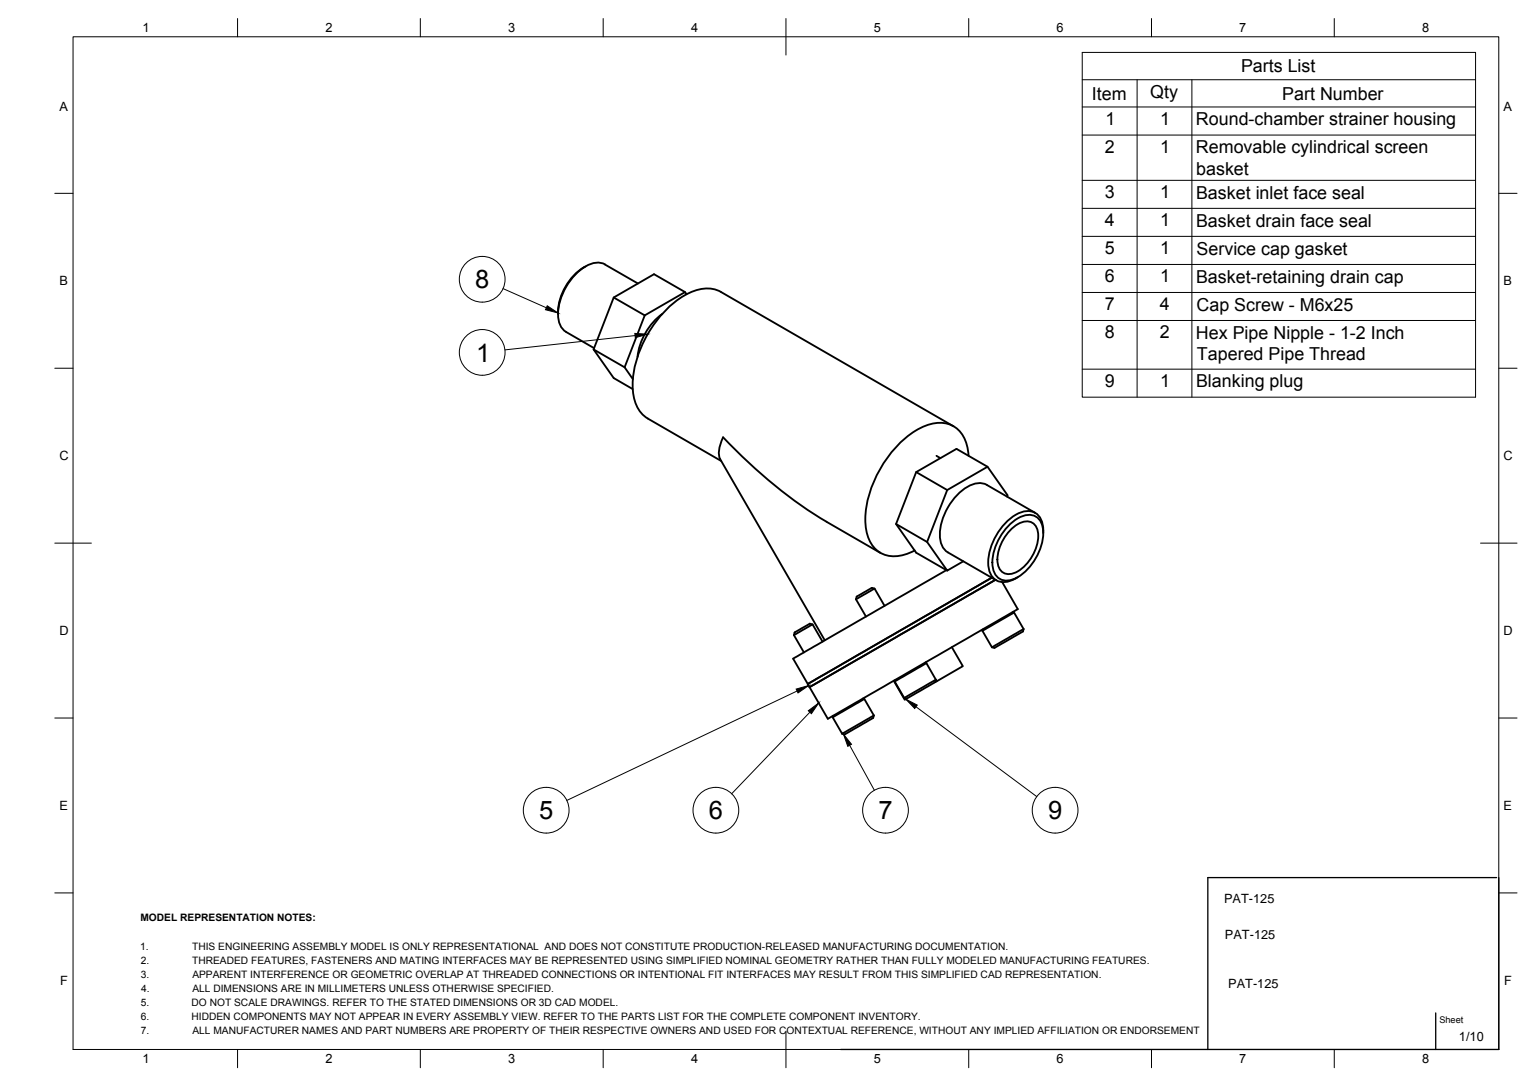
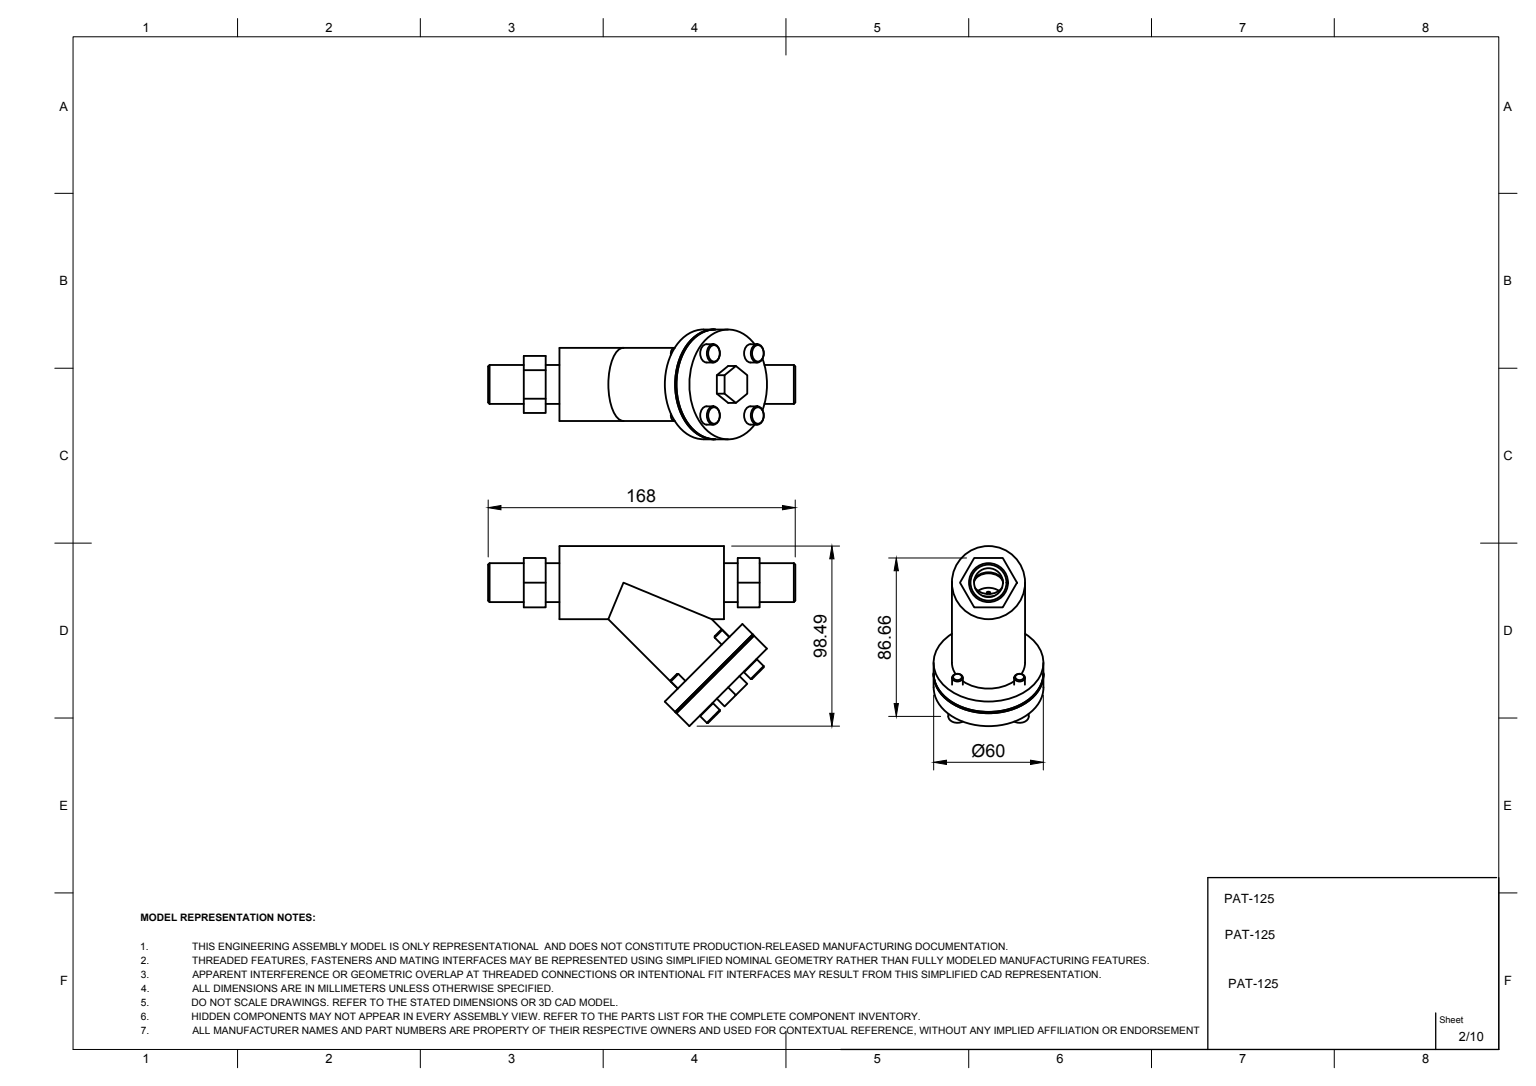
ISO-10303-21;
HEADER;
/* Generated by software containing ST-Developer
 * from STEP Tools, Inc. (www.steptools.com) 
 */

FILE_DESCRIPTION(
/* description */ ('Y-strainer with drain'),
/* implementation_level */ '2;1');

FILE_NAME(
/* name */ 'PAT-125',
/* time_stamp */ '2026-10-28T00:41:55-07:00',
/* author */ (''),
/* organization */ (''),
/* preprocessor_version */ 'ST-DEVELOPER v20.2',
/* originating_system */ 'Autodesk Translation Framework v15.17.0.0',
/* authorisation */ '');

FILE_SCHEMA (('AUTOMOTIVE_DESIGN { 1 0 10303 214 3 1 1 }'));
ENDSEC;

DATA;
#10=MECHANICAL_DESIGN_GEOMETRIC_PRESENTATION_REPRESENTATION('',(#93,#94,
#95,#96,#97,#98,#99,#100,#101),#8864);
#11=ITEM_DEFINED_TRANSFORMATION($,$,#3495,#3757);
#12=ITEM_DEFINED_TRANSFORMATION($,$,#3557,#3758);
#13=ITEM_DEFINED_TRANSFORMATION($,$,#3630,#3759);
#14=ITEM_DEFINED_TRANSFORMATION($,$,#3639,#3760);
#15=ITEM_DEFINED_TRANSFORMATION($,$,#3648,#3761);
#16=ITEM_DEFINED_TRANSFORMATION($,$,#3669,#3762);
#17=ITEM_DEFINED_TRANSFORMATION($,$,#3694,#3763);
#18=ITEM_DEFINED_TRANSFORMATION($,$,#3694,#3764);
#19=ITEM_DEFINED_TRANSFORMATION($,$,#3694,#3765);
#20=ITEM_DEFINED_TRANSFORMATION($,$,#3694,#3766);
#21=ITEM_DEFINED_TRANSFORMATION($,$,#3720,#3767);
#22=ITEM_DEFINED_TRANSFORMATION($,$,#3720,#3768);
#23=ITEM_DEFINED_TRANSFORMATION($,$,#3744,#3769);
#24=ITEM_DEFINED_TRANSFORMATION($,$,#3494,#3770);
#25=(
REPRESENTATION_RELATIONSHIP($,$,#8907,#8906)
REPRESENTATION_RELATIONSHIP_WITH_TRANSFORMATION(#11)
SHAPE_REPRESENTATION_RELATIONSHIP()
);
#26=(
REPRESENTATION_RELATIONSHIP($,$,#8908,#8906)
REPRESENTATION_RELATIONSHIP_WITH_TRANSFORMATION(#12)
SHAPE_REPRESENTATION_RELATIONSHIP()
);
#27=(
REPRESENTATION_RELATIONSHIP($,$,#8909,#8906)
REPRESENTATION_RELATIONSHIP_WITH_TRANSFORMATION(#13)
SHAPE_REPRESENTATION_RELATIONSHIP()
);
#28=(
REPRESENTATION_RELATIONSHIP($,$,#8910,#8906)
REPRESENTATION_RELATIONSHIP_WITH_TRANSFORMATION(#14)
SHAPE_REPRESENTATION_RELATIONSHIP()
);
#29=(
REPRESENTATION_RELATIONSHIP($,$,#8911,#8906)
REPRESENTATION_RELATIONSHIP_WITH_TRANSFORMATION(#15)
SHAPE_REPRESENTATION_RELATIONSHIP()
);
#30=(
REPRESENTATION_RELATIONSHIP($,$,#8912,#8906)
REPRESENTATION_RELATIONSHIP_WITH_TRANSFORMATION(#16)
SHAPE_REPRESENTATION_RELATIONSHIP()
);
#31=(
REPRESENTATION_RELATIONSHIP($,$,#8913,#8906)
REPRESENTATION_RELATIONSHIP_WITH_TRANSFORMATION(#17)
SHAPE_REPRESENTATION_RELATIONSHIP()
);
#32=(
REPRESENTATION_RELATIONSHIP($,$,#8913,#8906)
REPRESENTATION_RELATIONSHIP_WITH_TRANSFORMATION(#18)
SHAPE_REPRESENTATION_RELATIONSHIP()
);
#33=(
REPRESENTATION_RELATIONSHIP($,$,#8913,#8906)
REPRESENTATION_RELATIONSHIP_WITH_TRANSFORMATION(#19)
SHAPE_REPRESENTATION_RELATIONSHIP()
);
#34=(
REPRESENTATION_RELATIONSHIP($,$,#8913,#8906)
REPRESENTATION_RELATIONSHIP_WITH_TRANSFORMATION(#20)
SHAPE_REPRESENTATION_RELATIONSHIP()
);
#35=(
REPRESENTATION_RELATIONSHIP($,$,#8914,#8906)
REPRESENTATION_RELATIONSHIP_WITH_TRANSFORMATION(#21)
SHAPE_REPRESENTATION_RELATIONSHIP()
);
#36=(
REPRESENTATION_RELATIONSHIP($,$,#8914,#8906)
REPRESENTATION_RELATIONSHIP_WITH_TRANSFORMATION(#22)
SHAPE_REPRESENTATION_RELATIONSHIP()
);
#37=(
REPRESENTATION_RELATIONSHIP($,$,#8915,#8906)
REPRESENTATION_RELATIONSHIP_WITH_TRANSFORMATION(#23)
SHAPE_REPRESENTATION_RELATIONSHIP()
);
#38=(
REPRESENTATION_RELATIONSHIP($,$,#8906,#8905)
REPRESENTATION_RELATIONSHIP_WITH_TRANSFORMATION(#24)
SHAPE_REPRESENTATION_RELATIONSHIP()
);
#39=CONTEXT_DEPENDENT_SHAPE_REPRESENTATION(#25,#8891);
#40=CONTEXT_DEPENDENT_SHAPE_REPRESENTATION(#26,#8892);
#41=CONTEXT_DEPENDENT_SHAPE_REPRESENTATION(#27,#8893);
#42=CONTEXT_DEPENDENT_SHAPE_REPRESENTATION(#28,#8894);
#43=CONTEXT_DEPENDENT_SHAPE_REPRESENTATION(#29,#8895);
#44=CONTEXT_DEPENDENT_SHAPE_REPRESENTATION(#30,#8896);
#45=CONTEXT_DEPENDENT_SHAPE_REPRESENTATION(#31,#8897);
#46=CONTEXT_DEPENDENT_SHAPE_REPRESENTATION(#32,#8898);
#47=CONTEXT_DEPENDENT_SHAPE_REPRESENTATION(#33,#8899);
#48=CONTEXT_DEPENDENT_SHAPE_REPRESENTATION(#34,#8900);
#49=CONTEXT_DEPENDENT_SHAPE_REPRESENTATION(#35,#8901);
#50=CONTEXT_DEPENDENT_SHAPE_REPRESENTATION(#36,#8902);
#51=CONTEXT_DEPENDENT_SHAPE_REPRESENTATION(#37,#8903);
#52=CONTEXT_DEPENDENT_SHAPE_REPRESENTATION(#38,#8904);
#53=NEXT_ASSEMBLY_USAGE_OCCURRENCE('Round-chamber strainer housing:1',
'Round-chamber strainer housing:1','Round-chamber strainer housing:1',#8918,
#8919,'Round-chamber strainer housing:1');
#54=NEXT_ASSEMBLY_USAGE_OCCURRENCE(
'Removable cylindrical screen basket:1',
'Removable cylindrical screen basket:1',
'Removable cylindrical screen basket:1',#8918,#8920,
'Removable cylindrical screen basket:1');
#55=NEXT_ASSEMBLY_USAGE_OCCURRENCE('Basket inlet face seal:1',
'Basket inlet face seal:1','Basket inlet face seal:1',#8918,#8921,
'Basket inlet face seal:1');
#56=NEXT_ASSEMBLY_USAGE_OCCURRENCE('Basket drain face seal:1',
'Basket drain face seal:1','Basket drain face seal:1',#8918,#8922,
'Basket drain face seal:1');
#57=NEXT_ASSEMBLY_USAGE_OCCURRENCE('Service cap gasket:1',
'Service cap gasket:1','Service cap gasket:1',#8918,#8923,
'Service cap gasket:1');
#58=NEXT_ASSEMBLY_USAGE_OCCURRENCE('Basket-retaining drain cap:1',
'Basket-retaining drain cap:1','Basket-retaining drain cap:1',#8918,#8924,
'Basket-retaining drain cap:1');
#59=NEXT_ASSEMBLY_USAGE_OCCURRENCE('Cap Screw - M6x25:2',
'Cap Screw - M6x25:2','Cap Screw - M6x25:2',#8918,#8925,
'Cap Screw - M6x25:2');
#60=NEXT_ASSEMBLY_USAGE_OCCURRENCE('Cap Screw - M6x25:3',
'Cap Screw - M6x25:3','Cap Screw - M6x25:3',#8918,#8925,
'Cap Screw - M6x25:3');
#61=NEXT_ASSEMBLY_USAGE_OCCURRENCE('Cap Screw - M6x25:4',
'Cap Screw - M6x25:4','Cap Screw - M6x25:4',#8918,#8925,
'Cap Screw - M6x25:4');
#62=NEXT_ASSEMBLY_USAGE_OCCURRENCE('Cap Screw - M6x25:5',
'Cap Screw - M6x25:5','Cap Screw - M6x25:5',#8918,#8925,
'Cap Screw - M6x25:5');
#63=NEXT_ASSEMBLY_USAGE_OCCURRENCE(
'Hex Pipe Nipple - 1-2 Inch Tapered Pipe Thread:2',
'Hex Pipe Nipple - 1-2 Inch Tapered Pipe Thread:2',
'Hex Pipe Nipple - 1-2 Inch Tapered Pipe Thread:2',#8918,#8926,
'Hex Pipe Nipple - 1-2 Inch Tapered Pipe Thread:2');
#64=NEXT_ASSEMBLY_USAGE_OCCURRENCE(
'Hex Pipe Nipple - 1-2 Inch Tapered Pipe Thread:3',
'Hex Pipe Nipple - 1-2 Inch Tapered Pipe Thread:3',
'Hex Pipe Nipple - 1-2 Inch Tapered Pipe Thread:3',#8918,#8926,
'Hex Pipe Nipple - 1-2 Inch Tapered Pipe Thread:3');
#65=NEXT_ASSEMBLY_USAGE_OCCURRENCE('Blanking plug:2','Blanking plug:2',
'Blanking plug:2',#8918,#8927,'Blanking plug:2');
#66=NEXT_ASSEMBLY_USAGE_OCCURRENCE(
'Strainer housing basket seals cap and fittings:1',
'Strainer housing basket seals cap and fittings:1',
'Strainer housing basket seals cap and fittings:1',#8917,#8918,
'Strainer housing basket seals cap and fittings:1');
#67=ORIENTED_CLOSED_SHELL('',*,#3390,.F.);
#68=CONICAL_SURFACE('',#3697,0.475,0.785398163397449);
#69=CONICAL_SURFACE('',#3701,0.485,0.785398163397448);
#70=CONICAL_SURFACE('',#3705,0.31,0.463647609000806);
#71=CONICAL_SURFACE('',#3709,0.27,0.785398163397448);
#72=CONICAL_SURFACE('',#3736,1.025,0.785398163397448);
#73=CONICAL_SURFACE('',#3739,1.025,0.785398163397448);
#74=BREP_WITH_VOIDS('Body1',#3389,(#67));
#75=SHAPE_REPRESENTATION_RELATIONSHIP('SRR','None',#8907,#84);
#76=SHAPE_REPRESENTATION_RELATIONSHIP('SRR','None',#8908,#85);
#77=SHAPE_REPRESENTATION_RELATIONSHIP('SRR','None',#8909,#86);
#78=SHAPE_REPRESENTATION_RELATIONSHIP('SRR','None',#8910,#87);
#79=SHAPE_REPRESENTATION_RELATIONSHIP('SRR','None',#8911,#88);
#80=SHAPE_REPRESENTATION_RELATIONSHIP('SRR','None',#8912,#89);
#81=SHAPE_REPRESENTATION_RELATIONSHIP('SRR','None',#8913,#90);
#82=SHAPE_REPRESENTATION_RELATIONSHIP('SRR','None',#8914,#91);
#83=SHAPE_REPRESENTATION_RELATIONSHIP('SRR','None',#8915,#92);
#84=ADVANCED_BREP_SHAPE_REPRESENTATION('',(#102),#8855);
#85=ADVANCED_BREP_SHAPE_REPRESENTATION('',(#103),#8856);
#86=ADVANCED_BREP_SHAPE_REPRESENTATION('',(#104),#8857);
#87=ADVANCED_BREP_SHAPE_REPRESENTATION('',(#105),#8858);
#88=ADVANCED_BREP_SHAPE_REPRESENTATION('',(#106),#8859);
#89=ADVANCED_BREP_SHAPE_REPRESENTATION('',(#107),#8860);
#90=ADVANCED_BREP_SHAPE_REPRESENTATION('',(#74),#8861);
#91=ADVANCED_BREP_SHAPE_REPRESENTATION('',(#108),#8862);
#92=ADVANCED_BREP_SHAPE_REPRESENTATION('',(#109),#8863);
#93=STYLED_ITEM('',(#9012),#102);
#94=STYLED_ITEM('',(#9026),#103);
#95=STYLED_ITEM('',(#9040),#104);
#96=STYLED_ITEM('',(#9040),#105);
#97=STYLED_ITEM('',(#9019),#106);
#98=STYLED_ITEM('',(#9019),#107);
#99=STYLED_ITEM('',(#9040),#74);
#100=STYLED_ITEM('',(#9019),#108);
#101=STYLED_ITEM('',(#9047),#109);
#102=MANIFOLD_SOLID_BREP('Body1',#3383);
#103=MANIFOLD_SOLID_BREP('Body1',#3384);
#104=MANIFOLD_SOLID_BREP('Body1',#3385);
#105=MANIFOLD_SOLID_BREP('Body1',#3386);
#106=MANIFOLD_SOLID_BREP('Body1',#3387);
#107=MANIFOLD_SOLID_BREP('Body1',#3388);
#108=MANIFOLD_SOLID_BREP('Body1',#3391);
#109=MANIFOLD_SOLID_BREP('Body1',#3392);
#110=B_SPLINE_CURVE_WITH_KNOTS('',3,(#4530,#4531,#4532,#4533,#4534,#4535,
#4536,#4537,#4538,#4539,#4540,#4541,#4542,#4543,#4544,#4545,#4546,#4547,
#4548,#4549),.UNSPECIFIED.,.F.,.F.,(4,2,2,2,2,2,2,2,2,4),(-4.14934014091753,
-3.99654801890952,-3.81097439305959,-3.62540076720966,-3.2542535155098,
-2.75110698726675,-2.2479604590237,-1.9375436083893,-1.7823351830721,-1.6271267577549),
 .UNSPECIFIED.);
#111=B_SPLINE_CURVE_WITH_KNOTS('',3,(#4550,#4551,#4552,#4553,#4554,#4555,
#4556,#4557,#4558,#4559,#4560,#4561,#4562,#4563,#4564,#4565,#4566,#4567,
#4568,#4569,#4570),.UNSPECIFIED.,.F.,.F.,(4,2,2,2,2,3,2,2,2,4),(-1.6271267577549,
-1.4719183324377,-1.3167099071205,-1.00629305648611,-0.503146528243052,
0.,0.371147251699857,0.556720877549785,0.742294503399713,0.895086625004965),
 .UNSPECIFIED.);
#112=B_SPLINE_CURVE_WITH_KNOTS('',3,(#4581,#4582,#4583,#4584,#4585,#4586,
#4587,#4588,#4589,#4590),.UNSPECIFIED.,.F.,.F.,(4,2,2,2,4),(1.74412062919654,
1.93171537626907,2.23482107464905,2.53792677302904,2.72552152010157),
 .UNSPECIFIED.);
#113=B_SPLINE_CURVE_WITH_KNOTS('',3,(#4608,#4609,#4610,#4611,#4612,#4613,
#4614,#4615,#4616,#4617,#4618,#4619,#4620,#4621,#4622,#4623,#4624,#4625,
#4626),.UNSPECIFIED.,.F.,.F.,(4,2,2,2,2,3,2,2,4),(-1.08793576529359,-1.02464359039736,
-0.589129183459348,-0.223538305364611,-0.111769152682306,0.,0.0571948520978316,
0.114389704195663,0.138769598257235),.UNSPECIFIED.);
#114=B_SPLINE_CURVE_WITH_KNOTS('',3,(#4628,#4629,#4630,#4631,#4632,#4633,
#4634,#4635,#4636,#4637,#4638,#4639,#4640,#4641,#4642,#4643,#4644,#4645),
 .UNSPECIFIED.,.F.,.F.,(4,2,2,2,2,2,2,2,4),(2.32433792360818,2.34871781766975,
2.40591266976758,2.46310752186541,2.57487667454772,2.68664582723002,3.05223670532476,
3.48775111226277,3.551043287159),.UNSPECIFIED.);
#115=B_SPLINE_CURVE_WITH_KNOTS('',3,(#4698,#4699,#4700,#4701,#4702,#4703,
#4704,#4705,#4706,#4707),.UNSPECIFIED.,.F.,.F.,(4,2,2,2,4),(0.,0.0376910486946462,
0.0753820973892924,0.113073058602025,0.150764019814758),.UNSPECIFIED.);
#116=B_SPLINE_CURVE_WITH_KNOTS('',3,(#4708,#4709,#4710,#4711,#4712,#4713,
#4714,#4715,#4716,#4717,#4718,#4719,#4720,#4721,#4722,#4723,#4724,#4725,
#4726,#4727,#4728,#4729,#4730,#4731,#4732,#4733),.UNSPECIFIED.,.F.,.F.,
(4,2,2,2,2,2,2,2,2,2,2,2,4),(0.150764019814758,0.188454981027491,0.226145942240224,
0.26383699093487,0.301528039629516,0.339219088324162,0.376910137018808,
0.414601098231541,0.452292059444274,0.489983020657007,0.527673981869739,
0.565365030564385,0.603056079259032),.UNSPECIFIED.);
#117=B_SPLINE_CURVE_WITH_KNOTS('',3,(#4737,#4738,#4739,#4740,#4741,#4742,
#4743,#4744,#4745,#4746,#4747,#4748,#4749,#4750,#4751,#4752,#4753,#4754,
#4755,#4756,#4757,#4758,#4759,#4760,#4761,#4762),.UNSPECIFIED.,.F.,.F.,
(4,2,2,2,2,2,2,2,2,2,2,2,4),(0.,0.0376957822030297,0.0753915644060595,0.113087218301784,
0.150782872197509,0.188478526093234,0.226174179988958,0.263869962191988,
0.301565744395018,0.339261526598047,0.376957308801077,0.414652962696802,
0.452348616592527),.UNSPECIFIED.);
#118=B_SPLINE_CURVE_WITH_KNOTS('',3,(#4763,#4764,#4765,#4766,#4767,#4768,
#4769,#4770,#4771,#4772),.UNSPECIFIED.,.F.,.F.,(4,2,2,2,4),(0.452348616592527,
0.490044270488251,0.527739924383976,0.565435706587006,0.603131488790035),
 .UNSPECIFIED.);
#119=B_SPLINE_CURVE_WITH_KNOTS('',3,(#4776,#4777,#4778,#4779,#4780,#4781,
#4782,#4783,#4784,#4785),.UNSPECIFIED.,.F.,.F.,(4,2,2,2,4),(0.,0.0376957822030298,
0.0753915644060595,0.113087218301784,0.150782872197509),.UNSPECIFIED.);
#120=B_SPLINE_CURVE_WITH_KNOTS('',3,(#4786,#4787,#4788,#4789,#4790,#4791,
#4792,#4793,#4794,#4795,#4796,#4797,#4798,#4799,#4800,#4801,#4802,#4803,
#4804,#4805,#4806,#4807,#4808,#4809,#4810,#4811),.UNSPECIFIED.,.F.,.F.,
(4,2,2,2,2,2,2,2,2,2,2,2,4),(0.150782872197509,0.188478526093234,0.226174179988958,
0.263869962191988,0.301565744395018,0.339261526598047,0.376957308801077,
0.414652962696802,0.452348616592526,0.490044270488251,0.527739924383976,
0.565435706587005,0.603131488790035),.UNSPECIFIED.);
#121=B_SPLINE_CURVE_WITH_KNOTS('',3,(#4815,#4816,#4817,#4818,#4819,#4820,
#4821,#4822,#4823,#4824,#4825,#4826,#4827,#4828,#4829,#4830,#4831,#4832,
#4833,#4834,#4835,#4836,#4837,#4838,#4839,#4840),.UNSPECIFIED.,.F.,.F.,
(4,2,2,2,2,2,2,2,2,2,2,2,4),(0.,0.0376910486946462,0.0753820973892924,0.113073058602025,
0.150764019814758,0.188454981027491,0.226145942240224,0.26383699093487,
0.301528039629516,0.339219088324162,0.376910137018808,0.414601098231541,
0.452292059444274),.UNSPECIFIED.);
#122=B_SPLINE_CURVE_WITH_KNOTS('',3,(#4841,#4842,#4843,#4844,#4845,#4846,
#4847,#4848,#4849,#4850),.UNSPECIFIED.,.F.,.F.,(4,2,2,2,4),(0.452292059444274,
0.489983020657006,0.527673981869739,0.565365030564385,0.603056079259032),
 .UNSPECIFIED.);
#123=B_SPLINE_CURVE_WITH_KNOTS('',3,(#4854,#4855,#4856,#4857,#4858,#4859,
#4860,#4861,#4862,#4863),.UNSPECIFIED.,.F.,.F.,(4,2,2,2,4),(0.,0.0376910486946458,
0.0753820973892915,0.113073058602024,0.150764019814757),.UNSPECIFIED.);
#124=B_SPLINE_CURVE_WITH_KNOTS('',3,(#4864,#4865,#4866,#4867,#4868,#4869,
#4870,#4871,#4872,#4873,#4874,#4875,#4876,#4877,#4878,#4879,#4880,#4881,
#4882,#4883,#4884,#4885,#4886,#4887,#4888,#4889),.UNSPECIFIED.,.F.,.F.,
(4,2,2,2,2,2,2,2,2,2,2,2,4),(0.150764019814757,0.18845498102749,0.226145942240223,
0.263836990934869,0.301528039629515,0.339219088324161,0.376910137018807,
0.41460109823154,0.452292059444273,0.489983020657006,0.527673981869738,
0.565365030564384,0.603056079259031),.UNSPECIFIED.);
#125=B_SPLINE_CURVE_WITH_KNOTS('',3,(#4893,#4894,#4895,#4896,#4897,#4898,
#4899,#4900,#4901,#4902,#4903,#4904,#4905,#4906,#4907,#4908,#4909,#4910,
#4911,#4912,#4913,#4914,#4915,#4916,#4917,#4918),.UNSPECIFIED.,.F.,.F.,
(4,2,2,2,2,2,2,2,2,2,2,2,4),(0.,0.0376957822030297,0.0753915644060595,0.113087218301784,
0.150782872197509,0.188478526093234,0.226174179988958,0.263869962191988,
0.301565744395018,0.339261526598047,0.376957308801077,0.414652962696802,
0.452348616592527),.UNSPECIFIED.);
#126=B_SPLINE_CURVE_WITH_KNOTS('',3,(#4919,#4920,#4921,#4922,#4923,#4924,
#4925,#4926,#4927,#4928),.UNSPECIFIED.,.F.,.F.,(4,2,2,2,4),(0.452348616592527,
0.490044270488251,0.527739924383976,0.565435706587006,0.603131488790035),
 .UNSPECIFIED.);
#127=B_SPLINE_CURVE_WITH_KNOTS('',3,(#4932,#4933,#4934,#4935,#4936,#4937,
#4938,#4939,#4940,#4941),.UNSPECIFIED.,.F.,.F.,(4,2,2,2,4),(0.,0.0376957822030298,
0.0753915644060595,0.113087218301784,0.150782872197509),.UNSPECIFIED.);
#128=B_SPLINE_CURVE_WITH_KNOTS('',3,(#4942,#4943,#4944,#4945,#4946,#4947,
#4948,#4949,#4950,#4951,#4952,#4953,#4954,#4955,#4956,#4957,#4958,#4959,
#4960,#4961,#4962,#4963,#4964,#4965,#4966,#4967),.UNSPECIFIED.,.F.,.F.,
(4,2,2,2,2,2,2,2,2,2,2,2,4),(0.150782872197509,0.188478526093234,0.226174179988958,
0.263869962191988,0.301565744395018,0.339261526598047,0.376957308801077,
0.414652962696802,0.452348616592526,0.490044270488251,0.527739924383976,
0.565435706587005,0.603131488790035),.UNSPECIFIED.);
#129=B_SPLINE_CURVE_WITH_KNOTS('',3,(#4971,#4972,#4973,#4974,#4975,#4976,
#4977,#4978,#4979,#4980,#4981,#4982,#4983,#4984,#4985,#4986,#4987,#4988,
#4989,#4990,#4991,#4992,#4993,#4994,#4995,#4996),.UNSPECIFIED.,.F.,.F.,
(4,2,2,2,2,2,2,2,2,2,2,2,4),(0.,0.0376910486946462,0.0753820973892924,0.113073058602025,
0.150764019814758,0.188454981027491,0.226145942240224,0.26383699093487,
0.301528039629516,0.339219088324161,0.376910137018807,0.41460109823154,
0.452292059444273),.UNSPECIFIED.);
#130=B_SPLINE_CURVE_WITH_KNOTS('',3,(#4997,#4998,#4999,#5000,#5001,#5002,
#5003,#5004,#5005,#5006),.UNSPECIFIED.,.F.,.F.,(4,2,2,2,4),(0.452292059444273,
0.489983020657006,0.527673981869739,0.565365030564385,0.603056079259031),
 .UNSPECIFIED.);
#131=B_SPLINE_CURVE_WITH_KNOTS('',3,(#5010,#5011,#5012,#5013,#5014,#5015,
#5016,#5017,#5018,#5019),.UNSPECIFIED.,.F.,.F.,(4,2,2,2,4),(0.,0.0376910486946464,
0.0753820973892928,0.113073058602026,0.150764019814759),.UNSPECIFIED.);
#132=B_SPLINE_CURVE_WITH_KNOTS('',3,(#5020,#5021,#5022,#5023,#5024,#5025,
#5026,#5027,#5028,#5029,#5030,#5031,#5032,#5033,#5034,#5035,#5036,#5037,
#5038,#5039,#5040,#5041,#5042,#5043,#5044,#5045),.UNSPECIFIED.,.F.,.F.,
(4,2,2,2,2,2,2,2,2,2,2,2,4),(0.150764019814759,0.188454981027492,0.226145942240225,
0.263836990934871,0.301528039629517,0.339219088324163,0.37691013701881,
0.414601098231543,0.452292059444276,0.489983020657009,0.527673981869742,
0.565365030564388,0.603056079259034),.UNSPECIFIED.);
#133=B_SPLINE_CURVE_WITH_KNOTS('',3,(#5049,#5050,#5051,#5052,#5053,#5054,
#5055,#5056,#5057,#5058,#5059,#5060,#5061,#5062,#5063,#5064,#5065,#5066,
#5067,#5068,#5069,#5070,#5071,#5072,#5073,#5074),.UNSPECIFIED.,.F.,.F.,
(4,2,2,2,2,2,2,2,2,2,2,2,4),(0.,0.0376957822030297,0.0753915644060594,0.113087218301785,
0.15078287219751,0.188478526093235,0.22617417998896,0.26386996219199,0.301565744395019,
0.339261526598049,0.376957308801079,0.414652962696804,0.452348616592528),
 .UNSPECIFIED.);
#134=B_SPLINE_CURVE_WITH_KNOTS('',3,(#5075,#5076,#5077,#5078,#5079,#5080,
#5081,#5082,#5083,#5084),.UNSPECIFIED.,.F.,.F.,(4,2,2,2,4),(0.452348616592528,
0.490044270488253,0.527739924383978,0.565435706587008,0.603131488790038),
 .UNSPECIFIED.);
#135=B_SPLINE_CURVE_WITH_KNOTS('',3,(#5088,#5089,#5090,#5091,#5092,#5093,
#5094,#5095,#5096,#5097),.UNSPECIFIED.,.F.,.F.,(4,2,2,2,4),(0.,0.0376957822030298,
0.0753915644060595,0.113087218301784,0.150782872197509),.UNSPECIFIED.);
#136=B_SPLINE_CURVE_WITH_KNOTS('',3,(#5098,#5099,#5100,#5101,#5102,#5103,
#5104,#5105,#5106,#5107,#5108,#5109,#5110,#5111,#5112,#5113,#5114,#5115,
#5116,#5117,#5118,#5119,#5120,#5121,#5122,#5123),.UNSPECIFIED.,.F.,.F.,
(4,2,2,2,2,2,2,2,2,2,2,2,4),(0.150782872197509,0.188478526093234,0.226174179988959,
0.263869962191988,0.301565744395018,0.339261526598048,0.376957308801078,
0.414652962696803,0.452348616592528,0.490044270488253,0.527739924383978,
0.565435706587008,0.603131488790038),.UNSPECIFIED.);
#137=B_SPLINE_CURVE_WITH_KNOTS('',3,(#5127,#5128,#5129,#5130,#5131,#5132,
#5133,#5134,#5135,#5136,#5137,#5138,#5139,#5140,#5141,#5142,#5143,#5144,
#5145,#5146,#5147,#5148,#5149,#5150,#5151,#5152),.UNSPECIFIED.,.F.,.F.,
(4,2,2,2,2,2,2,2,2,2,2,2,4),(0.,0.0376910486946464,0.0753820973892928,0.113073058602026,
0.150764019814759,0.188454981027492,0.226145942240225,0.263836990934871,
0.301528039629517,0.339219088324164,0.37691013701881,0.414601098231543,
0.452292059444276),.UNSPECIFIED.);
#138=B_SPLINE_CURVE_WITH_KNOTS('',3,(#5153,#5154,#5155,#5156,#5157,#5158,
#5159,#5160,#5161,#5162),.UNSPECIFIED.,.F.,.F.,(4,2,2,2,4),(0.452292059444276,
0.489983020657009,0.527673981869742,0.565365030564388,0.603056079259035),
 .UNSPECIFIED.);
#139=B_SPLINE_CURVE_WITH_KNOTS('',3,(#5166,#5167,#5168,#5169,#5170,#5171,
#5172,#5173,#5174,#5175),.UNSPECIFIED.,.F.,.F.,(4,2,2,2,4),(0.,0.0376910486946464,
0.0753820973892928,0.113073058602026,0.150764019814759),.UNSPECIFIED.);
#140=B_SPLINE_CURVE_WITH_KNOTS('',3,(#5176,#5177,#5178,#5179,#5180,#5181,
#5182,#5183,#5184,#5185,#5186,#5187,#5188,#5189,#5190,#5191,#5192,#5193,
#5194,#5195,#5196,#5197,#5198,#5199,#5200,#5201),.UNSPECIFIED.,.F.,.F.,
(4,2,2,2,2,2,2,2,2,2,2,2,4),(0.150764019814759,0.188454981027492,0.226145942240225,
0.263836990934871,0.301528039629517,0.339219088324163,0.376910137018809,
0.414601098231542,0.452292059444276,0.489983020657009,0.527673981869741,
0.565365030564388,0.603056079259034),.UNSPECIFIED.);
#141=B_SPLINE_CURVE_WITH_KNOTS('',3,(#5205,#5206,#5207,#5208,#5209,#5210,
#5211,#5212,#5213,#5214,#5215,#5216,#5217,#5218,#5219,#5220,#5221,#5222,
#5223,#5224,#5225,#5226,#5227,#5228,#5229,#5230),.UNSPECIFIED.,.F.,.F.,
(4,2,2,2,2,2,2,2,2,2,2,2,4),(0.,0.0376957822030297,0.0753915644060595,0.113087218301784,
0.150782872197509,0.188478526093234,0.226174179988959,0.263869962191989,
0.301565744395019,0.339261526598048,0.376957308801078,0.414652962696803,
0.452348616592528),.UNSPECIFIED.);
#142=B_SPLINE_CURVE_WITH_KNOTS('',3,(#5231,#5232,#5233,#5234,#5235,#5236,
#5237,#5238,#5239,#5240),.UNSPECIFIED.,.F.,.F.,(4,2,2,2,4),(0.452348616592528,
0.490044270488253,0.527739924383978,0.565435706587008,0.603131488790038),
 .UNSPECIFIED.);
#143=B_SPLINE_CURVE_WITH_KNOTS('',3,(#5244,#5245,#5246,#5247,#5248,#5249,
#5250,#5251,#5252,#5253),.UNSPECIFIED.,.F.,.F.,(4,2,2,2,4),(0.,0.03769578220303,
0.0753915644060599,0.113087218301785,0.15078287219751),.UNSPECIFIED.);
#144=B_SPLINE_CURVE_WITH_KNOTS('',3,(#5254,#5255,#5256,#5257,#5258,#5259,
#5260,#5261,#5262,#5263,#5264,#5265,#5266,#5267,#5268,#5269,#5270,#5271,
#5272,#5273,#5274,#5275,#5276,#5277,#5278,#5279),.UNSPECIFIED.,.F.,.F.,
(4,2,2,2,2,2,2,2,2,2,2,2,4),(0.15078287219751,0.188478526093235,0.22617417998896,
0.263869962191989,0.301565744395019,0.339261526598049,0.376957308801078,
0.414652962696803,0.452348616592528,0.490044270488253,0.527739924383978,
0.565435706587008,0.603131488790038),.UNSPECIFIED.);
#145=B_SPLINE_CURVE_WITH_KNOTS('',3,(#5283,#5284,#5285,#5286,#5287,#5288,
#5289,#5290,#5291,#5292,#5293,#5294,#5295,#5296,#5297,#5298,#5299,#5300,
#5301,#5302,#5303,#5304,#5305,#5306,#5307,#5308),.UNSPECIFIED.,.F.,.F.,
(4,2,2,2,2,2,2,2,2,2,2,2,4),(0.,0.0376910486946464,0.0753820973892928,0.113073058602026,
0.150764019814759,0.188454981027492,0.226145942240225,0.263836990934871,
0.301528039629517,0.339219088324163,0.37691013701881,0.414601098231543,
0.452292059444276),.UNSPECIFIED.);
#146=B_SPLINE_CURVE_WITH_KNOTS('',3,(#5309,#5310,#5311,#5312,#5313,#5314,
#5315,#5316,#5317,#5318),.UNSPECIFIED.,.F.,.F.,(4,2,2,2,4),(0.452292059444276,
0.489983020657009,0.527673981869742,0.565365030564388,0.603056079259034),
 .UNSPECIFIED.);
#147=B_SPLINE_CURVE_WITH_KNOTS('',3,(#5322,#5323,#5324,#5325,#5326,#5327,
#5328,#5329,#5330,#5331),.UNSPECIFIED.,.F.,.F.,(4,2,2,2,4),(0.,0.0376910486946463,
0.0753820973892926,0.113073058602026,0.150764019814759),.UNSPECIFIED.);
#148=B_SPLINE_CURVE_WITH_KNOTS('',3,(#5332,#5333,#5334,#5335,#5336,#5337,
#5338,#5339,#5340,#5341,#5342,#5343,#5344,#5345,#5346,#5347,#5348,#5349,
#5350,#5351,#5352,#5353,#5354,#5355,#5356,#5357),.UNSPECIFIED.,.F.,.F.,
(4,2,2,2,2,2,2,2,2,2,2,2,4),(0.150764019814759,0.188454981027492,0.226145942240225,
0.263836990934871,0.301528039629517,0.339219088324163,0.37691013701881,
0.414601098231543,0.452292059444276,0.489983020657009,0.527673981869742,
0.565365030564388,0.603056079259034),.UNSPECIFIED.);
#149=B_SPLINE_CURVE_WITH_KNOTS('',3,(#5361,#5362,#5363,#5364,#5365,#5366,
#5367,#5368,#5369,#5370,#5371,#5372,#5373,#5374,#5375,#5376,#5377,#5378,
#5379,#5380,#5381,#5382,#5383,#5384,#5385,#5386),.UNSPECIFIED.,.F.,.F.,
(4,2,2,2,2,2,2,2,2,2,2,2,4),(0.,0.0376957822030299,0.0753915644060597,0.113087218301785,
0.15078287219751,0.188478526093234,0.226174179988959,0.263869962191989,
0.301565744395019,0.339261526598049,0.376957308801079,0.414652962696804,
0.452348616592529),.UNSPECIFIED.);
#150=B_SPLINE_CURVE_WITH_KNOTS('',3,(#5387,#5388,#5389,#5390,#5391,#5392,
#5393,#5394,#5395,#5396),.UNSPECIFIED.,.F.,.F.,(4,2,2,2,4),(0.452348616592529,
0.490044270488253,0.527739924383978,0.565435706587008,0.603131488790038),
 .UNSPECIFIED.);
#151=B_SPLINE_CURVE_WITH_KNOTS('',3,(#5400,#5401,#5402,#5403,#5404,#5405,
#5406,#5407,#5408,#5409),.UNSPECIFIED.,.F.,.F.,(4,2,2,2,4),(0.,0.0376957822030298,
0.0753915644060597,0.113087218301785,0.150782872197509),.UNSPECIFIED.);
#152=B_SPLINE_CURVE_WITH_KNOTS('',3,(#5410,#5411,#5412,#5413,#5414,#5415,
#5416,#5417,#5418,#5419,#5420,#5421,#5422,#5423,#5424,#5425,#5426,#5427,
#5428,#5429,#5430,#5431,#5432,#5433,#5434,#5435),.UNSPECIFIED.,.F.,.F.,
(4,2,2,2,2,2,2,2,2,2,2,2,4),(0.150782872197509,0.188478526093234,0.226174179988959,
0.263869962191989,0.301565744395019,0.339261526598049,0.376957308801079,
0.414652962696804,0.452348616592528,0.490044270488253,0.527739924383978,
0.565435706587008,0.603131488790038),.UNSPECIFIED.);
#153=B_SPLINE_CURVE_WITH_KNOTS('',3,(#5439,#5440,#5441,#5442,#5443,#5444,
#5445,#5446,#5447,#5448,#5449,#5450,#5451,#5452,#5453,#5454,#5455,#5456,
#5457,#5458,#5459,#5460,#5461,#5462,#5463,#5464),.UNSPECIFIED.,.F.,.F.,
(4,2,2,2,2,2,2,2,2,2,2,2,4),(0.,0.0376910486946463,0.0753820973892926,0.113073058602025,
0.150764019814758,0.188454981027491,0.226145942240224,0.263836990934871,
0.301528039629517,0.339219088324163,0.37691013701881,0.414601098231543,
0.452292059444276),.UNSPECIFIED.);
#154=B_SPLINE_CURVE_WITH_KNOTS('',3,(#5465,#5466,#5467,#5468,#5469,#5470,
#5471,#5472,#5473,#5474),.UNSPECIFIED.,.F.,.F.,(4,2,2,2,4),(0.452292059444276,
0.489983020657009,0.527673981869742,0.565365030564388,0.603056079259034),
 .UNSPECIFIED.);
#155=B_SPLINE_CURVE_WITH_KNOTS('',3,(#5478,#5479,#5480,#5481,#5482,#5483,
#5484,#5485,#5486,#5487),.UNSPECIFIED.,.F.,.F.,(4,2,2,2,4),(0.,0.0376910486946462,
0.0753820973892924,0.113073058602025,0.150764019814758),.UNSPECIFIED.);
#156=B_SPLINE_CURVE_WITH_KNOTS('',3,(#5488,#5489,#5490,#5491,#5492,#5493,
#5494,#5495,#5496,#5497,#5498,#5499,#5500,#5501,#5502,#5503,#5504,#5505,
#5506,#5507,#5508,#5509,#5510,#5511,#5512,#5513),.UNSPECIFIED.,.F.,.F.,
(4,2,2,2,2,2,2,2,2,2,2,2,4),(0.150764019814758,0.188454981027491,0.226145942240224,
0.26383699093487,0.301528039629516,0.339219088324162,0.376910137018808,
0.414601098231541,0.452292059444274,0.489983020657007,0.527673981869739,
0.565365030564385,0.603056079259032),.UNSPECIFIED.);
#157=B_SPLINE_CURVE_WITH_KNOTS('',3,(#5517,#5518,#5519,#5520,#5521,#5522,
#5523,#5524,#5525,#5526,#5527,#5528,#5529,#5530,#5531,#5532,#5533,#5534,
#5535,#5536,#5537,#5538,#5539,#5540,#5541,#5542),.UNSPECIFIED.,.F.,.F.,
(4,2,2,2,2,2,2,2,2,2,2,2,4),(0.,0.0376957822030297,0.0753915644060595,0.113087218301784,
0.150782872197509,0.188478526093234,0.226174179988958,0.263869962191988,
0.301565744395018,0.339261526598047,0.376957308801077,0.414652962696802,
0.452348616592527),.UNSPECIFIED.);
#158=B_SPLINE_CURVE_WITH_KNOTS('',3,(#5543,#5544,#5545,#5546,#5547,#5548,
#5549,#5550,#5551,#5552),.UNSPECIFIED.,.F.,.F.,(4,2,2,2,4),(0.452348616592527,
0.490044270488251,0.527739924383976,0.565435706587006,0.603131488790035),
 .UNSPECIFIED.);
#159=B_SPLINE_CURVE_WITH_KNOTS('',3,(#5556,#5557,#5558,#5559,#5560,#5561,
#5562,#5563,#5564,#5565),.UNSPECIFIED.,.F.,.F.,(4,2,2,2,4),(0.,0.0376957822030298,
0.0753915644060595,0.113087218301784,0.150782872197509),.UNSPECIFIED.);
#160=B_SPLINE_CURVE_WITH_KNOTS('',3,(#5566,#5567,#5568,#5569,#5570,#5571,
#5572,#5573,#5574,#5575,#5576,#5577,#5578,#5579,#5580,#5581,#5582,#5583,
#5584,#5585,#5586,#5587,#5588,#5589,#5590,#5591),.UNSPECIFIED.,.F.,.F.,
(4,2,2,2,2,2,2,2,2,2,2,2,4),(0.150782872197509,0.188478526093234,0.226174179988958,
0.263869962191988,0.301565744395018,0.339261526598047,0.376957308801077,
0.414652962696802,0.452348616592526,0.490044270488251,0.527739924383976,
0.565435706587005,0.603131488790035),.UNSPECIFIED.);
#161=B_SPLINE_CURVE_WITH_KNOTS('',3,(#5595,#5596,#5597,#5598,#5599,#5600,
#5601,#5602,#5603,#5604,#5605,#5606,#5607,#5608,#5609,#5610,#5611,#5612,
#5613,#5614,#5615,#5616,#5617,#5618,#5619,#5620),.UNSPECIFIED.,.F.,.F.,
(4,2,2,2,2,2,2,2,2,2,2,2,4),(0.,0.0376910486946462,0.0753820973892924,0.113073058602025,
0.150764019814758,0.188454981027491,0.226145942240224,0.26383699093487,
0.301528039629516,0.339219088324162,0.376910137018808,0.414601098231541,
0.452292059444274),.UNSPECIFIED.);
#162=B_SPLINE_CURVE_WITH_KNOTS('',3,(#5621,#5622,#5623,#5624,#5625,#5626,
#5627,#5628,#5629,#5630),.UNSPECIFIED.,.F.,.F.,(4,2,2,2,4),(0.452292059444274,
0.489983020657006,0.527673981869739,0.565365030564385,0.603056079259032),
 .UNSPECIFIED.);
#163=B_SPLINE_CURVE_WITH_KNOTS('',3,(#5634,#5635,#5636,#5637,#5638,#5639,
#5640,#5641,#5642,#5643),.UNSPECIFIED.,.F.,.F.,(4,2,2,2,4),(0.,0.0376910486946462,
0.0753820973892923,0.113073058602025,0.150764019814758),.UNSPECIFIED.);
#164=B_SPLINE_CURVE_WITH_KNOTS('',3,(#5644,#5645,#5646,#5647,#5648,#5649,
#5650,#5651,#5652,#5653,#5654,#5655,#5656,#5657,#5658,#5659,#5660,#5661,
#5662,#5663,#5664,#5665,#5666,#5667,#5668,#5669),.UNSPECIFIED.,.F.,.F.,
(4,2,2,2,2,2,2,2,2,2,2,2,4),(0.150764019814758,0.188454981027491,0.226145942240223,
0.26383699093487,0.301528039629516,0.339219088324162,0.376910137018808,
0.414601098231541,0.452292059444274,0.489983020657007,0.527673981869739,
0.565365030564386,0.603056079259032),.UNSPECIFIED.);
#165=B_SPLINE_CURVE_WITH_KNOTS('',3,(#5673,#5674,#5675,#5676,#5677,#5678,
#5679,#5680,#5681,#5682,#5683,#5684,#5685,#5686,#5687,#5688,#5689,#5690,
#5691,#5692,#5693,#5694,#5695,#5696,#5697,#5698),.UNSPECIFIED.,.F.,.F.,
(4,2,2,2,2,2,2,2,2,2,2,2,4),(0.,0.0376957822030297,0.0753915644060595,0.113087218301784,
0.150782872197509,0.188478526093234,0.226174179988958,0.263869962191988,
0.301565744395018,0.339261526598047,0.376957308801077,0.414652962696802,
0.452348616592527),.UNSPECIFIED.);
#166=B_SPLINE_CURVE_WITH_KNOTS('',3,(#5699,#5700,#5701,#5702,#5703,#5704,
#5705,#5706,#5707,#5708),.UNSPECIFIED.,.F.,.F.,(4,2,2,2,4),(0.452348616592527,
0.490044270488251,0.527739924383976,0.565435706587006,0.603131488790035),
 .UNSPECIFIED.);
#167=B_SPLINE_CURVE_WITH_KNOTS('',3,(#5712,#5713,#5714,#5715,#5716,#5717,
#5718,#5719,#5720,#5721),.UNSPECIFIED.,.F.,.F.,(4,2,2,2,4),(0.,0.0376957822030297,
0.0753915644060595,0.113087218301784,0.150782872197509),.UNSPECIFIED.);
#168=B_SPLINE_CURVE_WITH_KNOTS('',3,(#5722,#5723,#5724,#5725,#5726,#5727,
#5728,#5729,#5730,#5731,#5732,#5733,#5734,#5735,#5736,#5737,#5738,#5739,
#5740,#5741,#5742,#5743,#5744,#5745,#5746,#5747),.UNSPECIFIED.,.F.,.F.,
(4,2,2,2,2,2,2,2,2,2,2,2,4),(0.150782872197509,0.188478526093234,0.226174179988958,
0.263869962191988,0.301565744395018,0.339261526598047,0.376957308801077,
0.414652962696802,0.452348616592527,0.490044270488251,0.527739924383976,
0.565435706587006,0.603131488790035),.UNSPECIFIED.);
#169=B_SPLINE_CURVE_WITH_KNOTS('',3,(#5751,#5752,#5753,#5754,#5755,#5756,
#5757,#5758,#5759,#5760,#5761,#5762,#5763,#5764,#5765,#5766,#5767,#5768,
#5769,#5770,#5771,#5772,#5773,#5774,#5775,#5776),.UNSPECIFIED.,.F.,.F.,
(4,2,2,2,2,2,2,2,2,2,2,2,4),(0.,0.0376910486946462,0.0753820973892923,0.113073058602025,
0.150764019814758,0.188454981027491,0.226145942240223,0.26383699093487,
0.301528039629516,0.339219088324162,0.376910137018808,0.414601098231541,
0.452292059444274),.UNSPECIFIED.);
#170=B_SPLINE_CURVE_WITH_KNOTS('',3,(#5777,#5778,#5779,#5780,#5781,#5782,
#5783,#5784,#5785,#5786),.UNSPECIFIED.,.F.,.F.,(4,2,2,2,4),(0.452292059444274,
0.489983020657007,0.527673981869739,0.565365030564386,0.603056079259032),
 .UNSPECIFIED.);
#171=B_SPLINE_CURVE_WITH_KNOTS('',3,(#5790,#5791,#5792,#5793,#5794,#5795,
#5796,#5797,#5798,#5799),.UNSPECIFIED.,.F.,.F.,(4,2,2,2,4),(0.,0.0376910486946457,
0.0753820973892915,0.113073058602024,0.150764019814757),.UNSPECIFIED.);
#172=B_SPLINE_CURVE_WITH_KNOTS('',3,(#5800,#5801,#5802,#5803,#5804,#5805,
#5806,#5807,#5808,#5809,#5810,#5811,#5812,#5813,#5814,#5815,#5816,#5817,
#5818,#5819,#5820,#5821,#5822,#5823,#5824,#5825),.UNSPECIFIED.,.F.,.F.,
(4,2,2,2,2,2,2,2,2,2,2,2,4),(0.150764019814757,0.18845498102749,0.226145942240223,
0.263836990934869,0.301528039629515,0.339219088324161,0.376910137018807,
0.41460109823154,0.452292059444273,0.489983020657006,0.527673981869738,
0.565365030564385,0.603056079259031),.UNSPECIFIED.);
#173=B_SPLINE_CURVE_WITH_KNOTS('',3,(#5829,#5830,#5831,#5832,#5833,#5834,
#5835,#5836,#5837,#5838,#5839,#5840,#5841,#5842,#5843,#5844,#5845,#5846,
#5847,#5848,#5849,#5850,#5851,#5852,#5853,#5854),.UNSPECIFIED.,.F.,.F.,
(4,2,2,2,2,2,2,2,2,2,2,2,4),(0.,0.0376957822030297,0.0753915644060595,0.113087218301784,
0.150782872197509,0.188478526093234,0.226174179988958,0.263869962191988,
0.301565744395018,0.339261526598047,0.376957308801077,0.414652962696802,
0.452348616592527),.UNSPECIFIED.);
#174=B_SPLINE_CURVE_WITH_KNOTS('',3,(#5855,#5856,#5857,#5858,#5859,#5860,
#5861,#5862,#5863,#5864),.UNSPECIFIED.,.F.,.F.,(4,2,2,2,4),(0.452348616592527,
0.490044270488251,0.527739924383976,0.565435706587006,0.603131488790035),
 .UNSPECIFIED.);
#175=B_SPLINE_CURVE_WITH_KNOTS('',3,(#5868,#5869,#5870,#5871,#5872,#5873,
#5874,#5875,#5876,#5877),.UNSPECIFIED.,.F.,.F.,(4,2,2,2,4),(0.,0.0376957822030297,
0.0753915644060595,0.113087218301784,0.150782872197509),.UNSPECIFIED.);
#176=B_SPLINE_CURVE_WITH_KNOTS('',3,(#5878,#5879,#5880,#5881,#5882,#5883,
#5884,#5885,#5886,#5887,#5888,#5889,#5890,#5891,#5892,#5893,#5894,#5895,
#5896,#5897,#5898,#5899,#5900,#5901,#5902,#5903),.UNSPECIFIED.,.F.,.F.,
(4,2,2,2,2,2,2,2,2,2,2,2,4),(0.150782872197509,0.188478526093234,0.226174179988958,
0.263869962191988,0.301565744395018,0.339261526598047,0.376957308801077,
0.414652962696802,0.452348616592527,0.490044270488251,0.527739924383976,
0.565435706587006,0.603131488790035),.UNSPECIFIED.);
#177=B_SPLINE_CURVE_WITH_KNOTS('',3,(#5907,#5908,#5909,#5910,#5911,#5912,
#5913,#5914,#5915,#5916,#5917,#5918,#5919,#5920,#5921,#5922,#5923,#5924,
#5925,#5926,#5927,#5928,#5929,#5930,#5931,#5932),.UNSPECIFIED.,.F.,.F.,
(4,2,2,2,2,2,2,2,2,2,2,2,4),(0.,0.0376910486946462,0.0753820973892923,0.113073058602025,
0.150764019814758,0.188454981027491,0.226145942240223,0.26383699093487,
0.301528039629516,0.339219088324162,0.376910137018807,0.41460109823154,
0.452292059444273),.UNSPECIFIED.);
#178=B_SPLINE_CURVE_WITH_KNOTS('',3,(#5933,#5934,#5935,#5936,#5937,#5938,
#5939,#5940,#5941,#5942),.UNSPECIFIED.,.F.,.F.,(4,2,2,2,4),(0.452292059444273,
0.489983020657006,0.527673981869739,0.565365030564385,0.603056079259031),
 .UNSPECIFIED.);
#179=B_SPLINE_CURVE_WITH_KNOTS('',3,(#5946,#5947,#5948,#5949,#5950,#5951,
#5952,#5953,#5954,#5955),.UNSPECIFIED.,.F.,.F.,(4,2,2,2,4),(0.,0.0376910486946459,
0.0753820973892919,0.113073058602025,0.150764019814758),.UNSPECIFIED.);
#180=B_SPLINE_CURVE_WITH_KNOTS('',3,(#5956,#5957,#5958,#5959,#5960,#5961,
#5962,#5963,#5964,#5965,#5966,#5967,#5968,#5969,#5970,#5971,#5972,#5973,
#5974,#5975,#5976,#5977,#5978,#5979,#5980,#5981),.UNSPECIFIED.,.F.,.F.,
(4,2,2,2,2,2,2,2,2,2,2,2,4),(0.150764019814758,0.188454981027491,0.226145942240224,
0.26383699093487,0.301528039629516,0.339219088324162,0.376910137018808,
0.414601098231541,0.452292059444274,0.489983020657007,0.52767398186974,
0.565365030564386,0.603056079259033),.UNSPECIFIED.);
#181=B_SPLINE_CURVE_WITH_KNOTS('',3,(#5985,#5986,#5987,#5988,#5989,#5990,
#5991,#5992,#5993,#5994,#5995,#5996,#5997,#5998,#5999,#6000,#6001,#6002,
#6003,#6004,#6005,#6006,#6007,#6008,#6009,#6010),.UNSPECIFIED.,.F.,.F.,
(4,2,2,2,2,2,2,2,2,2,2,2,4),(0.,0.0376957822030297,0.0753915644060594,0.113087218301785,
0.15078287219751,0.188478526093235,0.22617417998896,0.26386996219199,0.301565744395019,
0.339261526598049,0.376957308801079,0.414652962696804,0.452348616592528),
 .UNSPECIFIED.);
#182=B_SPLINE_CURVE_WITH_KNOTS('',3,(#6011,#6012,#6013,#6014,#6015,#6016,
#6017,#6018,#6019,#6020),.UNSPECIFIED.,.F.,.F.,(4,2,2,2,4),(0.452348616592528,
0.490044270488253,0.527739924383978,0.565435706587008,0.603131488790037),
 .UNSPECIFIED.);
#183=B_SPLINE_CURVE_WITH_KNOTS('',3,(#6024,#6025,#6026,#6027,#6028,#6029,
#6030,#6031,#6032,#6033),.UNSPECIFIED.,.F.,.F.,(4,2,2,2,4),(0.,0.0376957822030298,
0.0753915644060595,0.113087218301784,0.150782872197509),.UNSPECIFIED.);
#184=B_SPLINE_CURVE_WITH_KNOTS('',3,(#6034,#6035,#6036,#6037,#6038,#6039,
#6040,#6041,#6042,#6043,#6044,#6045,#6046,#6047,#6048,#6049,#6050,#6051,
#6052,#6053,#6054,#6055,#6056,#6057,#6058,#6059),.UNSPECIFIED.,.F.,.F.,
(4,2,2,2,2,2,2,2,2,2,2,2,4),(0.150782872197509,0.188478526093234,0.226174179988959,
0.263869962191988,0.301565744395018,0.339261526598048,0.376957308801077,
0.414652962696803,0.452348616592528,0.490044270488253,0.527739924383978,
0.565435706587008,0.603131488790037),.UNSPECIFIED.);
#185=B_SPLINE_CURVE_WITH_KNOTS('',3,(#6063,#6064,#6065,#6066,#6067,#6068,
#6069,#6070,#6071,#6072,#6073,#6074,#6075,#6076,#6077,#6078,#6079,#6080,
#6081,#6082,#6083,#6084,#6085,#6086,#6087,#6088),.UNSPECIFIED.,.F.,.F.,
(4,2,2,2,2,2,2,2,2,2,2,2,4),(0.,0.0376910486946464,0.0753820973892928,0.113073058602026,
0.150764019814759,0.188454981027492,0.226145942240225,0.263836990934871,
0.301528039629517,0.339219088324163,0.376910137018809,0.414601098231542,
0.452292059444275),.UNSPECIFIED.);
#186=B_SPLINE_CURVE_WITH_KNOTS('',3,(#6089,#6090,#6091,#6092,#6093,#6094,
#6095,#6096,#6097,#6098),.UNSPECIFIED.,.F.,.F.,(4,2,2,2,4),(0.452292059444275,
0.489983020657008,0.527673981869741,0.565365030564387,0.603056079259033),
 .UNSPECIFIED.);
#187=B_SPLINE_CURVE_WITH_KNOTS('',3,(#6102,#6103,#6104,#6105,#6106,#6107,
#6108,#6109,#6110,#6111),.UNSPECIFIED.,.F.,.F.,(4,2,2,2,4),(0.,0.0376910486946462,
0.0753820973892924,0.113073058602025,0.150764019814758),.UNSPECIFIED.);
#188=B_SPLINE_CURVE_WITH_KNOTS('',3,(#6112,#6113,#6114,#6115,#6116,#6117,
#6118,#6119,#6120,#6121,#6122,#6123,#6124,#6125,#6126,#6127,#6128,#6129,
#6130,#6131,#6132,#6133,#6134,#6135,#6136,#6137),.UNSPECIFIED.,.F.,.F.,
(4,2,2,2,2,2,2,2,2,2,2,2,4),(0.150764019814758,0.188454981027491,0.226145942240224,
0.263836990934871,0.301528039629517,0.339219088324163,0.376910137018809,
0.414601098231543,0.452292059444276,0.489983020657008,0.527673981869741,
0.565365030564388,0.603056079259034),.UNSPECIFIED.);
#189=B_SPLINE_CURVE_WITH_KNOTS('',3,(#6141,#6142,#6143,#6144,#6145,#6146,
#6147,#6148,#6149,#6150,#6151,#6152,#6153,#6154,#6155,#6156,#6157,#6158,
#6159,#6160,#6161,#6162,#6163,#6164,#6165,#6166),.UNSPECIFIED.,.F.,.F.,
(4,2,2,2,2,2,2,2,2,2,2,2,4),(0.,0.0376957822030297,0.0753915644060595,0.113087218301784,
0.150782872197509,0.188478526093234,0.226174179988959,0.263869962191989,
0.301565744395019,0.339261526598048,0.376957308801078,0.414652962696803,
0.452348616592528),.UNSPECIFIED.);
#190=B_SPLINE_CURVE_WITH_KNOTS('',3,(#6167,#6168,#6169,#6170,#6171,#6172,
#6173,#6174,#6175,#6176),.UNSPECIFIED.,.F.,.F.,(4,2,2,2,4),(0.452348616592528,
0.490044270488253,0.527739924383978,0.565435706587008,0.603131488790038),
 .UNSPECIFIED.);
#191=B_SPLINE_CURVE_WITH_KNOTS('',3,(#6180,#6181,#6182,#6183,#6184,#6185,
#6186,#6187,#6188,#6189),.UNSPECIFIED.,.F.,.F.,(4,2,2,2,4),(0.,0.03769578220303,
0.0753915644060599,0.113087218301785,0.15078287219751),.UNSPECIFIED.);
#192=B_SPLINE_CURVE_WITH_KNOTS('',3,(#6190,#6191,#6192,#6193,#6194,#6195,
#6196,#6197,#6198,#6199,#6200,#6201,#6202,#6203,#6204,#6205,#6206,#6207,
#6208,#6209,#6210,#6211,#6212,#6213,#6214,#6215),.UNSPECIFIED.,.F.,.F.,
(4,2,2,2,2,2,2,2,2,2,2,2,4),(0.15078287219751,0.188478526093235,0.226174179988959,
0.263869962191989,0.301565744395019,0.339261526598049,0.376957308801078,
0.414652962696803,0.452348616592528,0.490044270488253,0.527739924383978,
0.565435706587008,0.603131488790038),.UNSPECIFIED.);
#193=B_SPLINE_CURVE_WITH_KNOTS('',3,(#6219,#6220,#6221,#6222,#6223,#6224,
#6225,#6226,#6227,#6228,#6229,#6230,#6231,#6232,#6233,#6234,#6235,#6236,
#6237,#6238,#6239,#6240,#6241,#6242,#6243,#6244),.UNSPECIFIED.,.F.,.F.,
(4,2,2,2,2,2,2,2,2,2,2,2,4),(0.,0.0376910486946464,0.0753820973892928,0.113073058602026,
0.150764019814759,0.188454981027492,0.226145942240225,0.263836990934871,
0.301528039629517,0.339219088324163,0.37691013701881,0.414601098231543,
0.452292059444276),.UNSPECIFIED.);
#194=B_SPLINE_CURVE_WITH_KNOTS('',3,(#6245,#6246,#6247,#6248,#6249,#6250,
#6251,#6252,#6253,#6254),.UNSPECIFIED.,.F.,.F.,(4,2,2,2,4),(0.452292059444276,
0.489983020657009,0.527673981869742,0.565365030564388,0.603056079259034),
 .UNSPECIFIED.);
#195=B_SPLINE_CURVE_WITH_KNOTS('',3,(#6258,#6259,#6260,#6261,#6262,#6263,
#6264,#6265,#6266,#6267),.UNSPECIFIED.,.F.,.F.,(4,2,2,2,4),(0.,0.0376910486946463,
0.0753820973892926,0.113073058602026,0.150764019814759),.UNSPECIFIED.);
#196=B_SPLINE_CURVE_WITH_KNOTS('',3,(#6268,#6269,#6270,#6271,#6272,#6273,
#6274,#6275,#6276,#6277,#6278,#6279,#6280,#6281,#6282,#6283,#6284,#6285,
#6286,#6287,#6288,#6289,#6290,#6291,#6292,#6293),.UNSPECIFIED.,.F.,.F.,
(4,2,2,2,2,2,2,2,2,2,2,2,4),(0.150764019814759,0.188454981027491,0.226145942240224,
0.263836990934871,0.301528039629517,0.339219088324163,0.376910137018809,
0.414601098231542,0.452292059444275,0.489983020657008,0.527673981869741,
0.565365030564388,0.603056079259034),.UNSPECIFIED.);
#197=B_SPLINE_CURVE_WITH_KNOTS('',3,(#6297,#6298,#6299,#6300,#6301,#6302,
#6303,#6304,#6305,#6306,#6307,#6308,#6309,#6310,#6311,#6312,#6313,#6314,
#6315,#6316,#6317,#6318,#6319,#6320,#6321,#6322),.UNSPECIFIED.,.F.,.F.,
(4,2,2,2,2,2,2,2,2,2,2,2,4),(0.,0.0376957822030298,0.0753915644060597,0.113087218301785,
0.150782872197509,0.188478526093234,0.226174179988959,0.263869962191989,
0.301565744395019,0.339261526598049,0.376957308801079,0.414652962696803,
0.452348616592528),.UNSPECIFIED.);
#198=B_SPLINE_CURVE_WITH_KNOTS('',3,(#6323,#6324,#6325,#6326,#6327,#6328,
#6329,#6330,#6331,#6332),.UNSPECIFIED.,.F.,.F.,(4,2,2,2,4),(0.452348616592528,
0.490044270488253,0.527739924383978,0.565435706587008,0.603131488790038),
 .UNSPECIFIED.);
#199=B_SPLINE_CURVE_WITH_KNOTS('',3,(#6336,#6337,#6338,#6339,#6340,#6341,
#6342,#6343,#6344,#6345),.UNSPECIFIED.,.F.,.F.,(4,2,2,2,4),(0.,0.0376957822030298,
0.0753915644060597,0.113087218301785,0.150782872197509),.UNSPECIFIED.);
#200=B_SPLINE_CURVE_WITH_KNOTS('',3,(#6346,#6347,#6348,#6349,#6350,#6351,
#6352,#6353,#6354,#6355,#6356,#6357,#6358,#6359,#6360,#6361,#6362,#6363,
#6364,#6365,#6366,#6367,#6368,#6369,#6370,#6371),.UNSPECIFIED.,.F.,.F.,
(4,2,2,2,2,2,2,2,2,2,2,2,4),(0.150782872197509,0.188478526093234,0.226174179988959,
0.263869962191989,0.301565744395019,0.339261526598049,0.376957308801079,
0.414652962696804,0.452348616592528,0.490044270488253,0.527739924383978,
0.565435706587008,0.603131488790038),.UNSPECIFIED.);
#201=B_SPLINE_CURVE_WITH_KNOTS('',3,(#6375,#6376,#6377,#6378,#6379,#6380,
#6381,#6382,#6383,#6384,#6385,#6386,#6387,#6388,#6389,#6390,#6391,#6392,
#6393,#6394,#6395,#6396,#6397,#6398,#6399,#6400),.UNSPECIFIED.,.F.,.F.,
(4,2,2,2,2,2,2,2,2,2,2,2,4),(0.,0.0376910486946463,0.0753820973892926,0.113073058602026,
0.150764019814759,0.188454981027492,0.226145942240224,0.263836990934871,
0.301528039629517,0.339219088324163,0.37691013701881,0.414601098231543,
0.452292059444276),.UNSPECIFIED.);
#202=B_SPLINE_CURVE_WITH_KNOTS('',3,(#6401,#6402,#6403,#6404,#6405,#6406,
#6407,#6408,#6409,#6410),.UNSPECIFIED.,.F.,.F.,(4,2,2,2,4),(0.452292059444276,
0.489983020657008,0.527673981869741,0.565365030564388,0.603056079259034),
 .UNSPECIFIED.);
#203=B_SPLINE_CURVE_WITH_KNOTS('',3,(#6414,#6415,#6416,#6417,#6418,#6419,
#6420,#6421,#6422,#6423),.UNSPECIFIED.,.F.,.F.,(4,2,2,2,4),(0.,0.0376910486946462,
0.0753820973892923,0.113073058602025,0.150764019814758),.UNSPECIFIED.);
#204=B_SPLINE_CURVE_WITH_KNOTS('',3,(#6424,#6425,#6426,#6427,#6428,#6429,
#6430,#6431,#6432,#6433,#6434,#6435,#6436,#6437,#6438,#6439,#6440,#6441,
#6442,#6443,#6444,#6445,#6446,#6447,#6448,#6449),.UNSPECIFIED.,.F.,.F.,
(4,2,2,2,2,2,2,2,2,2,2,2,4),(0.150764019814758,0.188454981027491,0.226145942240223,
0.26383699093487,0.301528039629516,0.339219088324162,0.376910137018808,
0.414601098231541,0.452292059444274,0.489983020657007,0.527673981869739,
0.565365030564386,0.603056079259032),.UNSPECIFIED.);
#205=B_SPLINE_CURVE_WITH_KNOTS('',3,(#6453,#6454,#6455,#6456,#6457,#6458,
#6459,#6460,#6461,#6462,#6463,#6464,#6465,#6466,#6467,#6468,#6469,#6470,
#6471,#6472,#6473,#6474,#6475,#6476,#6477,#6478),.UNSPECIFIED.,.F.,.F.,
(4,2,2,2,2,2,2,2,2,2,2,2,4),(0.,0.0376957822030297,0.0753915644060595,0.113087218301784,
0.150782872197509,0.188478526093234,0.226174179988958,0.263869962191988,
0.301565744395018,0.339261526598047,0.376957308801077,0.414652962696802,
0.452348616592527),.UNSPECIFIED.);
#206=B_SPLINE_CURVE_WITH_KNOTS('',3,(#6479,#6480,#6481,#6482,#6483,#6484,
#6485,#6486,#6487,#6488),.UNSPECIFIED.,.F.,.F.,(4,2,2,2,4),(0.452348616592527,
0.490044270488251,0.527739924383976,0.565435706587006,0.603131488790035),
 .UNSPECIFIED.);
#207=B_SPLINE_CURVE_WITH_KNOTS('',3,(#6492,#6493,#6494,#6495,#6496,#6497,
#6498,#6499,#6500,#6501),.UNSPECIFIED.,.F.,.F.,(4,2,2,2,4),(0.,0.0376957822030297,
0.0753915644060595,0.113087218301784,0.150782872197509),.UNSPECIFIED.);
#208=B_SPLINE_CURVE_WITH_KNOTS('',3,(#6502,#6503,#6504,#6505,#6506,#6507,
#6508,#6509,#6510,#6511,#6512,#6513,#6514,#6515,#6516,#6517,#6518,#6519,
#6520,#6521,#6522,#6523,#6524,#6525,#6526,#6527),.UNSPECIFIED.,.F.,.F.,
(4,2,2,2,2,2,2,2,2,2,2,2,4),(0.150782872197509,0.188478526093234,0.226174179988958,
0.263869962191988,0.301565744395018,0.339261526598047,0.376957308801077,
0.414652962696802,0.452348616592527,0.490044270488251,0.527739924383976,
0.565435706587006,0.603131488790035),.UNSPECIFIED.);
#209=B_SPLINE_CURVE_WITH_KNOTS('',3,(#6531,#6532,#6533,#6534,#6535,#6536,
#6537,#6538,#6539,#6540,#6541,#6542,#6543,#6544,#6545,#6546,#6547,#6548,
#6549,#6550,#6551,#6552,#6553,#6554,#6555,#6556),.UNSPECIFIED.,.F.,.F.,
(4,2,2,2,2,2,2,2,2,2,2,2,4),(0.,0.0376910486946462,0.0753820973892923,0.113073058602025,
0.150764019814758,0.188454981027491,0.226145942240223,0.26383699093487,
0.301528039629516,0.339219088324162,0.376910137018808,0.414601098231541,
0.452292059444274),.UNSPECIFIED.);
#210=B_SPLINE_CURVE_WITH_KNOTS('',3,(#6557,#6558,#6559,#6560,#6561,#6562,
#6563,#6564,#6565,#6566),.UNSPECIFIED.,.F.,.F.,(4,2,2,2,4),(0.452292059444274,
0.489983020657007,0.527673981869739,0.565365030564386,0.603056079259032),
 .UNSPECIFIED.);
#211=B_SPLINE_CURVE_WITH_KNOTS('',3,(#6570,#6571,#6572,#6573,#6574,#6575,
#6576,#6577,#6578,#6579),.UNSPECIFIED.,.F.,.F.,(4,2,2,2,4),(0.,0.0376910486946462,
0.0753820973892923,0.113073058602025,0.150764019814758),.UNSPECIFIED.);
#212=B_SPLINE_CURVE_WITH_KNOTS('',3,(#6580,#6581,#6582,#6583,#6584,#6585,
#6586,#6587,#6588,#6589,#6590,#6591,#6592,#6593,#6594,#6595,#6596,#6597,
#6598,#6599,#6600,#6601,#6602,#6603,#6604,#6605),.UNSPECIFIED.,.F.,.F.,
(4,2,2,2,2,2,2,2,2,2,2,2,4),(0.150764019814758,0.188454981027491,0.226145942240223,
0.26383699093487,0.301528039629516,0.339219088324162,0.376910137018808,
0.414601098231541,0.452292059444274,0.489983020657006,0.527673981869739,
0.565365030564386,0.603056079259032),.UNSPECIFIED.);
#213=B_SPLINE_CURVE_WITH_KNOTS('',3,(#6609,#6610,#6611,#6612,#6613,#6614,
#6615,#6616,#6617,#6618,#6619,#6620,#6621,#6622,#6623,#6624,#6625,#6626,
#6627,#6628,#6629,#6630,#6631,#6632,#6633,#6634),.UNSPECIFIED.,.F.,.F.,
(4,2,2,2,2,2,2,2,2,2,2,2,4),(0.,0.0376957822030297,0.0753915644060594,0.113087218301784,
0.150782872197509,0.188478526093234,0.226174179988958,0.263869962191988,
0.301565744395018,0.339261526598047,0.376957308801077,0.414652962696802,
0.452348616592527),.UNSPECIFIED.);
#214=B_SPLINE_CURVE_WITH_KNOTS('',3,(#6635,#6636,#6637,#6638,#6639,#6640,
#6641,#6642,#6643,#6644),.UNSPECIFIED.,.F.,.F.,(4,2,2,2,4),(0.452348616592527,
0.490044270488251,0.527739924383976,0.565435706587006,0.603131488790035),
 .UNSPECIFIED.);
#215=B_SPLINE_CURVE_WITH_KNOTS('',3,(#6648,#6649,#6650,#6651,#6652,#6653,
#6654,#6655,#6656,#6657),.UNSPECIFIED.,.F.,.F.,(4,2,2,2,4),(0.,0.0376957822030297,
0.0753915644060594,0.113087218301784,0.150782872197509),.UNSPECIFIED.);
#216=B_SPLINE_CURVE_WITH_KNOTS('',3,(#6658,#6659,#6660,#6661,#6662,#6663,
#6664,#6665,#6666,#6667,#6668,#6669,#6670,#6671,#6672,#6673,#6674,#6675,
#6676,#6677,#6678,#6679,#6680,#6681,#6682,#6683),.UNSPECIFIED.,.F.,.F.,
(4,2,2,2,2,2,2,2,2,2,2,2,4),(0.150782872197509,0.188478526093234,0.226174179988958,
0.263869962191988,0.301565744395018,0.339261526598047,0.376957308801077,
0.414652962696802,0.452348616592527,0.490044270488251,0.527739924383976,
0.565435706587006,0.603131488790036),.UNSPECIFIED.);
#217=B_SPLINE_CURVE_WITH_KNOTS('',3,(#6687,#6688,#6689,#6690,#6691,#6692,
#6693,#6694,#6695,#6696,#6697,#6698,#6699,#6700,#6701,#6702,#6703,#6704,
#6705,#6706,#6707,#6708,#6709,#6710,#6711,#6712),.UNSPECIFIED.,.F.,.F.,
(4,2,2,2,2,2,2,2,2,2,2,2,4),(0.,0.0376910486946461,0.0753820973892922,0.113073058602025,
0.150764019814758,0.188454981027491,0.226145942240223,0.26383699093487,
0.301528039629516,0.339219088324162,0.376910137018808,0.414601098231541,
0.452292059444274),.UNSPECIFIED.);
#218=B_SPLINE_CURVE_WITH_KNOTS('',3,(#6713,#6714,#6715,#6716,#6717,#6718,
#6719,#6720,#6721,#6722),.UNSPECIFIED.,.F.,.F.,(4,2,2,2,4),(0.452292059444274,
0.489983020657007,0.527673981869739,0.565365030564385,0.603056079259032),
 .UNSPECIFIED.);
#219=B_SPLINE_CURVE_WITH_KNOTS('',3,(#6726,#6727,#6728,#6729,#6730,#6731,
#6732,#6733,#6734,#6735),.UNSPECIFIED.,.F.,.F.,(4,2,2,2,4),(0.,0.0376910486946457,
0.0753820973892915,0.113073058602025,0.150764019814758),.UNSPECIFIED.);
#220=B_SPLINE_CURVE_WITH_KNOTS('',3,(#6736,#6737,#6738,#6739,#6740,#6741,
#6742,#6743,#6744,#6745,#6746,#6747,#6748,#6749,#6750,#6751,#6752,#6753,
#6754,#6755,#6756,#6757,#6758,#6759,#6760,#6761),.UNSPECIFIED.,.F.,.F.,
(4,2,2,2,2,2,2,2,2,2,2,2,4),(0.150764019814758,0.18845498102749,0.226145942240223,
0.263836990934869,0.301528039629515,0.339219088324161,0.376910137018807,
0.41460109823154,0.452292059444273,0.489983020657006,0.527673981869738,
0.565365030564385,0.603056079259031),.UNSPECIFIED.);
#221=B_SPLINE_CURVE_WITH_KNOTS('',3,(#6765,#6766,#6767,#6768,#6769,#6770,
#6771,#6772,#6773,#6774,#6775,#6776,#6777,#6778,#6779,#6780,#6781,#6782,
#6783,#6784,#6785,#6786,#6787,#6788,#6789,#6790),.UNSPECIFIED.,.F.,.F.,
(4,2,2,2,2,2,2,2,2,2,2,2,4),(0.,0.0376957822030297,0.0753915644060594,0.113087218301784,
0.150782872197509,0.188478526093234,0.226174179988958,0.263869962191988,
0.301565744395018,0.339261526598047,0.376957308801077,0.414652962696802,
0.452348616592527),.UNSPECIFIED.);
#222=B_SPLINE_CURVE_WITH_KNOTS('',3,(#6791,#6792,#6793,#6794,#6795,#6796,
#6797,#6798,#6799,#6800),.UNSPECIFIED.,.F.,.F.,(4,2,2,2,4),(0.452348616592527,
0.490044270488251,0.527739924383976,0.565435706587006,0.603131488790035),
 .UNSPECIFIED.);
#223=B_SPLINE_CURVE_WITH_KNOTS('',3,(#6804,#6805,#6806,#6807,#6808,#6809,
#6810,#6811,#6812,#6813),.UNSPECIFIED.,.F.,.F.,(4,2,2,2,4),(0.,0.0376957822030297,
0.0753915644060594,0.113087218301784,0.150782872197509),.UNSPECIFIED.);
#224=B_SPLINE_CURVE_WITH_KNOTS('',3,(#6814,#6815,#6816,#6817,#6818,#6819,
#6820,#6821,#6822,#6823,#6824,#6825,#6826,#6827,#6828,#6829,#6830,#6831,
#6832,#6833,#6834,#6835,#6836,#6837,#6838,#6839),.UNSPECIFIED.,.F.,.F.,
(4,2,2,2,2,2,2,2,2,2,2,2,4),(0.150782872197509,0.188478526093234,0.226174179988958,
0.263869962191988,0.301565744395018,0.339261526598047,0.376957308801077,
0.414652962696802,0.452348616592527,0.490044270488251,0.527739924383976,
0.565435706587006,0.603131488790036),.UNSPECIFIED.);
#225=B_SPLINE_CURVE_WITH_KNOTS('',3,(#6843,#6844,#6845,#6846,#6847,#6848,
#6849,#6850,#6851,#6852,#6853,#6854,#6855,#6856,#6857,#6858,#6859,#6860,
#6861,#6862,#6863,#6864,#6865,#6866,#6867,#6868),.UNSPECIFIED.,.F.,.F.,
(4,2,2,2,2,2,2,2,2,2,2,2,4),(0.,0.0376910486946461,0.0753820973892922,0.113073058602025,
0.150764019814758,0.188454981027491,0.226145942240223,0.26383699093487,
0.301528039629516,0.339219088324162,0.376910137018807,0.41460109823154,
0.452292059444273),.UNSPECIFIED.);
#226=B_SPLINE_CURVE_WITH_KNOTS('',3,(#6869,#6870,#6871,#6872,#6873,#6874,
#6875,#6876,#6877,#6878),.UNSPECIFIED.,.F.,.F.,(4,2,2,2,4),(0.452292059444273,
0.489983020657006,0.527673981869739,0.565365030564385,0.603056079259031),
 .UNSPECIFIED.);
#227=B_SPLINE_CURVE_WITH_KNOTS('',3,(#6882,#6883,#6884,#6885,#6886,#6887,
#6888,#6889,#6890,#6891),.UNSPECIFIED.,.F.,.F.,(4,2,2,2,4),(0.,0.0376910486946459,
0.0753820973892918,0.113073058602025,0.150764019814758),.UNSPECIFIED.);
#228=B_SPLINE_CURVE_WITH_KNOTS('',3,(#6892,#6893,#6894,#6895,#6896,#6897,
#6898,#6899,#6900,#6901,#6902,#6903,#6904,#6905,#6906,#6907,#6908,#6909,
#6910,#6911,#6912,#6913,#6914,#6915,#6916,#6917),.UNSPECIFIED.,.F.,.F.,
(4,2,2,2,2,2,2,2,2,2,2,2,4),(0.150764019814758,0.188454981027491,0.226145942240224,
0.26383699093487,0.301528039629516,0.339219088324162,0.376910137018808,
0.414601098231541,0.452292059444274,0.489983020657007,0.52767398186974,
0.565365030564387,0.603056079259033),.UNSPECIFIED.);
#229=B_SPLINE_CURVE_WITH_KNOTS('',3,(#6921,#6922,#6923,#6924,#6925,#6926,
#6927,#6928,#6929,#6930,#6931,#6932,#6933,#6934,#6935,#6936,#6937,#6938,
#6939,#6940,#6941,#6942,#6943,#6944,#6945,#6946),.UNSPECIFIED.,.F.,.F.,
(4,2,2,2,2,2,2,2,2,2,2,2,4),(0.,0.0376957822030297,0.0753915644060594,0.113087218301785,
0.15078287219751,0.188478526093235,0.22617417998896,0.26386996219199,0.301565744395019,
0.339261526598049,0.376957308801079,0.414652962696804,0.452348616592528),
 .UNSPECIFIED.);
#230=B_SPLINE_CURVE_WITH_KNOTS('',3,(#6947,#6948,#6949,#6950,#6951,#6952,
#6953,#6954,#6955,#6956),.UNSPECIFIED.,.F.,.F.,(4,2,2,2,4),(0.452348616592528,
0.490044270488253,0.527739924383978,0.565435706587008,0.603131488790038),
 .UNSPECIFIED.);
#231=B_SPLINE_CURVE_WITH_KNOTS('',3,(#6960,#6961,#6962,#6963,#6964,#6965,
#6966,#6967,#6968,#6969),.UNSPECIFIED.,.F.,.F.,(4,2,2,2,4),(0.,0.0376957822030298,
0.0753915644060595,0.113087218301784,0.150782872197509),.UNSPECIFIED.);
#232=B_SPLINE_CURVE_WITH_KNOTS('',3,(#6970,#6971,#6972,#6973,#6974,#6975,
#6976,#6977,#6978,#6979,#6980,#6981,#6982,#6983,#6984,#6985,#6986,#6987,
#6988,#6989,#6990,#6991,#6992,#6993,#6994,#6995),.UNSPECIFIED.,.F.,.F.,
(4,2,2,2,2,2,2,2,2,2,2,2,4),(0.150782872197509,0.188478526093234,0.226174179988959,
0.263869962191988,0.301565744395018,0.339261526598048,0.376957308801078,
0.414652962696803,0.452348616592528,0.490044270488253,0.527739924383978,
0.565435706587008,0.603131488790037),.UNSPECIFIED.);
#233=B_SPLINE_CURVE_WITH_KNOTS('',3,(#6999,#7000,#7001,#7002,#7003,#7004,
#7005,#7006,#7007,#7008,#7009,#7010,#7011,#7012,#7013,#7014,#7015,#7016,
#7017,#7018,#7019,#7020,#7021,#7022,#7023,#7024),.UNSPECIFIED.,.F.,.F.,
(4,2,2,2,2,2,2,2,2,2,2,2,4),(0.,0.0376910486946464,0.0753820973892928,0.113073058602026,
0.150764019814759,0.188454981027492,0.226145942240225,0.263836990934871,
0.301528039629517,0.339219088324163,0.376910137018809,0.414601098231542,
0.452292059444275),.UNSPECIFIED.);
#234=B_SPLINE_CURVE_WITH_KNOTS('',3,(#7025,#7026,#7027,#7028,#7029,#7030,
#7031,#7032,#7033,#7034),.UNSPECIFIED.,.F.,.F.,(4,2,2,2,4),(0.452292059444275,
0.489983020657008,0.527673981869741,0.565365030564387,0.603056079259033),
 .UNSPECIFIED.);
#235=B_SPLINE_CURVE_WITH_KNOTS('',3,(#7038,#7039,#7040,#7041,#7042,#7043,
#7044,#7045,#7046,#7047),.UNSPECIFIED.,.F.,.F.,(4,2,2,2,4),(0.,0.0376910486946462,
0.0753820973892924,0.113073058602025,0.150764019814758),.UNSPECIFIED.);
#236=B_SPLINE_CURVE_WITH_KNOTS('',3,(#7048,#7049,#7050,#7051,#7052,#7053,
#7054,#7055,#7056,#7057,#7058,#7059,#7060,#7061,#7062,#7063,#7064,#7065,
#7066,#7067,#7068,#7069,#7070,#7071,#7072,#7073),.UNSPECIFIED.,.F.,.F.,
(4,2,2,2,2,2,2,2,2,2,2,2,4),(0.150764019814758,0.188454981027491,0.226145942240224,
0.263836990934871,0.301528039629517,0.339219088324163,0.376910137018809,
0.414601098231543,0.452292059444276,0.489983020657009,0.527673981869742,
0.565365030564388,0.603056079259034),.UNSPECIFIED.);
#237=B_SPLINE_CURVE_WITH_KNOTS('',3,(#7077,#7078,#7079,#7080,#7081,#7082,
#7083,#7084,#7085,#7086,#7087,#7088,#7089,#7090,#7091,#7092,#7093,#7094,
#7095,#7096,#7097,#7098,#7099,#7100,#7101,#7102),.UNSPECIFIED.,.F.,.F.,
(4,2,2,2,2,2,2,2,2,2,2,2,4),(0.,0.0376957822030297,0.0753915644060595,0.113087218301784,
0.150782872197509,0.188478526093234,0.226174179988959,0.263869962191989,
0.301565744395019,0.339261526598048,0.376957308801078,0.414652962696803,
0.452348616592528),.UNSPECIFIED.);
#238=B_SPLINE_CURVE_WITH_KNOTS('',3,(#7103,#7104,#7105,#7106,#7107,#7108,
#7109,#7110,#7111,#7112),.UNSPECIFIED.,.F.,.F.,(4,2,2,2,4),(0.452348616592528,
0.490044270488253,0.527739924383978,0.565435706587007,0.603131488790037),
 .UNSPECIFIED.);
#239=B_SPLINE_CURVE_WITH_KNOTS('',3,(#7116,#7117,#7118,#7119,#7120,#7121,
#7122,#7123,#7124,#7125),.UNSPECIFIED.,.F.,.F.,(4,2,2,2,4),(0.,0.03769578220303,
0.0753915644060599,0.113087218301785,0.15078287219751),.UNSPECIFIED.);
#240=B_SPLINE_CURVE_WITH_KNOTS('',3,(#7126,#7127,#7128,#7129,#7130,#7131,
#7132,#7133,#7134,#7135,#7136,#7137,#7138,#7139,#7140,#7141,#7142,#7143,
#7144,#7145,#7146,#7147,#7148,#7149,#7150,#7151),.UNSPECIFIED.,.F.,.F.,
(4,2,2,2,2,2,2,2,2,2,2,2,4),(0.15078287219751,0.188478526093235,0.22617417998896,
0.263869962191989,0.301565744395019,0.339261526598049,0.376957308801078,
0.414652962696803,0.452348616592528,0.490044270488253,0.527739924383978,
0.565435706587008,0.603131488790038),.UNSPECIFIED.);
#241=B_SPLINE_CURVE_WITH_KNOTS('',3,(#7155,#7156,#7157,#7158,#7159,#7160,
#7161,#7162,#7163,#7164,#7165,#7166,#7167,#7168,#7169,#7170,#7171,#7172,
#7173,#7174,#7175,#7176,#7177,#7178,#7179,#7180),.UNSPECIFIED.,.F.,.F.,
(4,2,2,2,2,2,2,2,2,2,2,2,4),(0.,0.0376910486946464,0.0753820973892928,0.113073058602026,
0.150764019814759,0.188454981027492,0.226145942240225,0.263836990934871,
0.301528039629517,0.339219088324164,0.37691013701881,0.414601098231543,
0.452292059444276),.UNSPECIFIED.);
#242=B_SPLINE_CURVE_WITH_KNOTS('',3,(#7181,#7182,#7183,#7184,#7185,#7186,
#7187,#7188,#7189,#7190),.UNSPECIFIED.,.F.,.F.,(4,2,2,2,4),(0.452292059444276,
0.489983020657009,0.527673981869742,0.565365030564388,0.603056079259034),
 .UNSPECIFIED.);
#243=B_SPLINE_CURVE_WITH_KNOTS('',3,(#7194,#7195,#7196,#7197,#7198,#7199,
#7200,#7201,#7202,#7203),.UNSPECIFIED.,.F.,.F.,(4,2,2,2,4),(0.,0.0376910486946463,
0.0753820973892926,0.113073058602026,0.150764019814759),.UNSPECIFIED.);
#244=B_SPLINE_CURVE_WITH_KNOTS('',3,(#7204,#7205,#7206,#7207,#7208,#7209,
#7210,#7211,#7212,#7213,#7214,#7215,#7216,#7217,#7218,#7219,#7220,#7221,
#7222,#7223,#7224,#7225,#7226,#7227,#7228,#7229),.UNSPECIFIED.,.F.,.F.,
(4,2,2,2,2,2,2,2,2,2,2,2,4),(0.150764019814759,0.188454981027492,0.226145942240224,
0.263836990934871,0.301528039629517,0.339219088324163,0.37691013701881,
0.414601098231543,0.452292059444276,0.489983020657009,0.527673981869742,
0.565365030564388,0.603056079259034),.UNSPECIFIED.);
#245=B_SPLINE_CURVE_WITH_KNOTS('',3,(#7233,#7234,#7235,#7236,#7237,#7238,
#7239,#7240,#7241,#7242,#7243,#7244,#7245,#7246,#7247,#7248,#7249,#7250,
#7251,#7252,#7253,#7254,#7255,#7256,#7257,#7258),.UNSPECIFIED.,.F.,.F.,
(4,2,2,2,2,2,2,2,2,2,2,2,4),(0.,0.0376957822030299,0.0753915644060597,0.113087218301785,
0.15078287219751,0.188478526093234,0.226174179988959,0.263869962191989,
0.301565744395019,0.339261526598049,0.376957308801079,0.414652962696804,
0.452348616592529),.UNSPECIFIED.);
#246=B_SPLINE_CURVE_WITH_KNOTS('',3,(#7259,#7260,#7261,#7262,#7263,#7264,
#7265,#7266,#7267,#7268),.UNSPECIFIED.,.F.,.F.,(4,2,2,2,4),(0.452348616592529,
0.490044270488253,0.527739924383978,0.565435706587008,0.603131488790038),
 .UNSPECIFIED.);
#247=B_SPLINE_CURVE_WITH_KNOTS('',3,(#7272,#7273,#7274,#7275,#7276,#7277,
#7278,#7279,#7280,#7281),.UNSPECIFIED.,.F.,.F.,(4,2,2,2,4),(0.,0.0376957822030299,
0.0753915644060597,0.113087218301785,0.15078287219751),.UNSPECIFIED.);
#248=B_SPLINE_CURVE_WITH_KNOTS('',3,(#7282,#7283,#7284,#7285,#7286,#7287,
#7288,#7289,#7290,#7291,#7292,#7293,#7294,#7295,#7296,#7297,#7298,#7299,
#7300,#7301,#7302,#7303,#7304,#7305,#7306,#7307),.UNSPECIFIED.,.F.,.F.,
(4,2,2,2,2,2,2,2,2,2,2,2,4),(0.15078287219751,0.188478526093234,0.226174179988959,
0.263869962191989,0.301565744395019,0.339261526598049,0.376957308801079,
0.414652962696804,0.452348616592529,0.490044270488253,0.527739924383978,
0.565435706587008,0.603131488790038),.UNSPECIFIED.);
#249=B_SPLINE_CURVE_WITH_KNOTS('',3,(#7311,#7312,#7313,#7314,#7315,#7316,
#7317,#7318,#7319,#7320,#7321,#7322,#7323,#7324,#7325,#7326,#7327,#7328,
#7329,#7330,#7331,#7332,#7333,#7334,#7335,#7336),.UNSPECIFIED.,.F.,.F.,
(4,2,2,2,2,2,2,2,2,2,2,2,4),(0.,0.0376910486946463,0.0753820973892926,0.113073058602026,
0.150764019814759,0.188454981027492,0.226145942240225,0.263836990934871,
0.301528039629517,0.339219088324163,0.37691013701881,0.414601098231543,
0.452292059444276),.UNSPECIFIED.);
#250=B_SPLINE_CURVE_WITH_KNOTS('',3,(#7337,#7338,#7339,#7340,#7341,#7342,
#7343,#7344,#7345,#7346),.UNSPECIFIED.,.F.,.F.,(4,2,2,2,4),(0.452292059444276,
0.489983020657008,0.527673981869741,0.565365030564388,0.603056079259034),
 .UNSPECIFIED.);
#251=B_SPLINE_CURVE_WITH_KNOTS('',3,(#7350,#7351,#7352,#7353,#7354,#7355,
#7356,#7357,#7358,#7359),.UNSPECIFIED.,.F.,.F.,(4,2,2,2,4),(0.,0.0376910486946462,
0.0753820973892923,0.113073058602025,0.150764019814758),.UNSPECIFIED.);
#252=B_SPLINE_CURVE_WITH_KNOTS('',3,(#7360,#7361,#7362,#7363,#7364,#7365,
#7366,#7367,#7368,#7369,#7370,#7371,#7372,#7373,#7374,#7375,#7376,#7377,
#7378,#7379,#7380,#7381,#7382,#7383,#7384,#7385),.UNSPECIFIED.,.F.,.F.,
(4,2,2,2,2,2,2,2,2,2,2,2,4),(0.150764019814758,0.188454981027491,0.226145942240223,
0.26383699093487,0.301528039629516,0.339219088324162,0.376910137018808,
0.414601098231541,0.452292059444274,0.489983020657006,0.527673981869739,
0.565365030564386,0.603056079259032),.UNSPECIFIED.);
#253=B_SPLINE_CURVE_WITH_KNOTS('',3,(#7389,#7390,#7391,#7392,#7393,#7394,
#7395,#7396,#7397,#7398,#7399,#7400,#7401,#7402,#7403,#7404,#7405,#7406,
#7407,#7408,#7409,#7410,#7411,#7412,#7413,#7414),.UNSPECIFIED.,.F.,.F.,
(4,2,2,2,2,2,2,2,2,2,2,2,4),(0.,0.0376957822030297,0.0753915644060594,0.113087218301784,
0.150782872197509,0.188478526093234,0.226174179988958,0.263869962191988,
0.301565744395018,0.339261526598047,0.376957308801077,0.414652962696802,
0.452348616592527),.UNSPECIFIED.);
#254=B_SPLINE_CURVE_WITH_KNOTS('',3,(#7415,#7416,#7417,#7418,#7419,#7420,
#7421,#7422,#7423,#7424),.UNSPECIFIED.,.F.,.F.,(4,2,2,2,4),(0.452348616592527,
0.490044270488251,0.527739924383976,0.565435706587006,0.603131488790035),
 .UNSPECIFIED.);
#255=B_SPLINE_CURVE_WITH_KNOTS('',3,(#7428,#7429,#7430,#7431,#7432,#7433,
#7434,#7435,#7436,#7437),.UNSPECIFIED.,.F.,.F.,(4,2,2,2,4),(0.,0.0376957822030297,
0.0753915644060594,0.113087218301784,0.150782872197509),.UNSPECIFIED.);
#256=B_SPLINE_CURVE_WITH_KNOTS('',3,(#7438,#7439,#7440,#7441,#7442,#7443,
#7444,#7445,#7446,#7447,#7448,#7449,#7450,#7451,#7452,#7453,#7454,#7455,
#7456,#7457,#7458,#7459,#7460,#7461,#7462,#7463),.UNSPECIFIED.,.F.,.F.,
(4,2,2,2,2,2,2,2,2,2,2,2,4),(0.150782872197509,0.188478526093234,0.226174179988958,
0.263869962191988,0.301565744395018,0.339261526598047,0.376957308801077,
0.414652962696802,0.452348616592527,0.490044270488251,0.527739924383976,
0.565435706587006,0.603131488790036),.UNSPECIFIED.);
#257=B_SPLINE_CURVE_WITH_KNOTS('',3,(#7467,#7468,#7469,#7470,#7471,#7472,
#7473,#7474,#7475,#7476,#7477,#7478,#7479,#7480,#7481,#7482,#7483,#7484,
#7485,#7486,#7487,#7488,#7489,#7490,#7491,#7492),.UNSPECIFIED.,.F.,.F.,
(4,2,2,2,2,2,2,2,2,2,2,2,4),(0.,0.0376910486946461,0.0753820973892922,0.113073058602025,
0.150764019814758,0.188454981027491,0.226145942240223,0.26383699093487,
0.301528039629516,0.339219088324162,0.376910137018808,0.414601098231541,
0.452292059444274),.UNSPECIFIED.);
#258=B_SPLINE_CURVE_WITH_KNOTS('',3,(#7493,#7494,#7495,#7496,#7497,#7498,
#7499,#7500,#7501,#7502),.UNSPECIFIED.,.F.,.F.,(4,2,2,2,4),(0.452292059444274,
0.489983020657007,0.527673981869739,0.565365030564385,0.603056079259032),
 .UNSPECIFIED.);
#259=B_SPLINE_CURVE_WITH_KNOTS('',3,(#7506,#7507,#7508,#7509,#7510,#7511,
#7512,#7513,#7514,#7515),.UNSPECIFIED.,.F.,.F.,(4,2,2,2,4),(0.,0.0376910486946462,
0.0753820973892923,0.113073058602025,0.150764019814758),.UNSPECIFIED.);
#260=B_SPLINE_CURVE_WITH_KNOTS('',3,(#7517,#7518,#7519,#7520,#7521,#7522,
#7523,#7524,#7525,#7526),.UNSPECIFIED.,.F.,.F.,(4,2,2,2,4),(0.452292059444274,
0.489983020657006,0.527673981869739,0.565365030564385,0.603056079259032),
 .UNSPECIFIED.);
#261=B_SPLINE_CURVE_WITH_KNOTS('',3,(#7527,#7528,#7529,#7530,#7531,#7532,
#7533,#7534,#7535,#7536,#7537,#7538,#7539,#7540,#7541,#7542,#7543,#7544),
 .UNSPECIFIED.,.F.,.F.,(4,2,2,2,2,2,2,2,4),(0.150764019814758,0.188454981027491,
0.226145942240223,0.26383699093487,0.301528039629516,0.339219088324162,
0.376910137018808,0.414601098231541,0.452292059444274),.UNSPECIFIED.);
#262=B_SPLINE_CURVE_WITH_KNOTS('',3,(#7548,#7549,#7550,#7551,#7552,#7553,
#7554,#7555,#7556,#7557,#7558,#7559,#7560,#7561,#7562,#7563,#7564,#7565),
 .UNSPECIFIED.,.F.,.F.,(4,2,2,2,2,2,2,2,4),(0.150782872197509,0.188478526093234,
0.226174179988958,0.263869962191988,0.301565744395018,0.339261526598047,
0.376957308801077,0.414652962696802,0.452348616592526),.UNSPECIFIED.);
#263=B_SPLINE_CURVE_WITH_KNOTS('',3,(#7567,#7568,#7569,#7570,#7571,#7572,
#7573,#7574,#7575,#7576),.UNSPECIFIED.,.F.,.F.,(4,2,2,2,4),(0.,0.0376957822030297,
0.0753915644060594,0.113087218301784,0.150782872197509),.UNSPECIFIED.);
#264=B_SPLINE_CURVE_WITH_KNOTS('',3,(#7577,#7578,#7579,#7580,#7581,#7582,
#7583,#7584,#7585,#7586),.UNSPECIFIED.,.F.,.F.,(4,2,2,2,4),(0.452348616592526,
0.490044270488251,0.527739924383976,0.565435706587006,0.603131488790035),
 .UNSPECIFIED.);
#265=B_SPLINE_CURVE_WITH_KNOTS('',3,(#7590,#7591,#7592,#7593,#7594,#7595,
#7596,#7597,#7598,#7599),.UNSPECIFIED.,.F.,.F.,(4,2,2,2,4),(0.,0.0376957822030297,
0.0753915644060594,0.113087218301784,0.150782872197509),.UNSPECIFIED.);
#266=B_SPLINE_CURVE_WITH_KNOTS('',3,(#7600,#7601,#7602,#7603,#7604,#7605,
#7606,#7607,#7608,#7609,#7610,#7611,#7612,#7613,#7614,#7615,#7616,#7617,
#7618,#7619,#7620,#7621,#7622,#7623,#7624,#7625),.UNSPECIFIED.,.F.,.F.,
(4,2,2,2,2,2,2,2,2,2,2,2,4),(0.150782872197509,0.188478526093234,0.226174179988958,
0.263869962191988,0.301565744395018,0.339261526598047,0.376957308801077,
0.414652962696802,0.452348616592527,0.490044270488251,0.527739924383976,
0.565435706587006,0.603131488790035),.UNSPECIFIED.);
#267=B_SPLINE_CURVE_WITH_KNOTS('',3,(#7629,#7630,#7631,#7632,#7633,#7634,
#7635,#7636,#7637,#7638,#7639,#7640,#7641,#7642,#7643,#7644,#7645,#7646,
#7647,#7648,#7649,#7650,#7651,#7652,#7653,#7654),.UNSPECIFIED.,.F.,.F.,
(4,2,2,2,2,2,2,2,2,2,2,2,4),(0.,0.0376910486946462,0.0753820973892923,0.113073058602025,
0.150764019814758,0.188454981027491,0.226145942240223,0.26383699093487,
0.301528039629516,0.339219088324162,0.376910137018808,0.414601098231541,
0.452292059444274),.UNSPECIFIED.);
#268=B_SPLINE_CURVE_WITH_KNOTS('',3,(#7655,#7656,#7657,#7658,#7659,#7660,
#7661,#7662,#7663,#7664),.UNSPECIFIED.,.F.,.F.,(4,2,2,2,4),(0.452292059444274,
0.489983020657006,0.527673981869739,0.565365030564385,0.603056079259032),
 .UNSPECIFIED.);
#269=B_SPLINE_CURVE_WITH_KNOTS('',3,(#7668,#7669,#7670,#7671,#7672,#7673,
#7674,#7675,#7676,#7677),.UNSPECIFIED.,.F.,.F.,(4,2,2,2,4),(0.,0.0376910486946457,
0.0753820973892915,0.113073058602024,0.150764019814757),.UNSPECIFIED.);
#270=B_SPLINE_CURVE_WITH_KNOTS('',3,(#7679,#7680,#7681,#7682,#7683,#7684,
#7685,#7686,#7687,#7688),.UNSPECIFIED.,.F.,.F.,(4,2,2,2,4),(0.452292059444273,
0.489983020657006,0.527673981869738,0.565365030564384,0.603056079259031),
 .UNSPECIFIED.);
#271=B_SPLINE_CURVE_WITH_KNOTS('',3,(#7689,#7690,#7691,#7692,#7693,#7694,
#7695,#7696,#7697,#7698,#7699,#7700,#7701,#7702,#7703,#7704,#7705,#7706),
 .UNSPECIFIED.,.F.,.F.,(4,2,2,2,2,2,2,2,4),(0.150764019814757,0.18845498102749,
0.226145942240223,0.263836990934869,0.301528039629515,0.339219088324161,
0.376910137018807,0.41460109823154,0.452292059444273),.UNSPECIFIED.);
#272=B_SPLINE_CURVE_WITH_KNOTS('',3,(#7710,#7711,#7712,#7713,#7714,#7715,
#7716,#7717,#7718,#7719,#7720,#7721,#7722,#7723,#7724,#7725,#7726,#7727),
 .UNSPECIFIED.,.F.,.F.,(4,2,2,2,2,2,2,2,4),(0.150782872197509,0.188478526093234,
0.226174179988958,0.263869962191988,0.301565744395018,0.339261526598047,
0.376957308801077,0.414652962696802,0.452348616592526),.UNSPECIFIED.);
#273=B_SPLINE_CURVE_WITH_KNOTS('',3,(#7729,#7730,#7731,#7732,#7733,#7734,
#7735,#7736,#7737,#7738),.UNSPECIFIED.,.F.,.F.,(4,2,2,2,4),(0.,0.0376957822030297,
0.0753915644060594,0.113087218301784,0.150782872197509),.UNSPECIFIED.);
#274=B_SPLINE_CURVE_WITH_KNOTS('',3,(#7739,#7740,#7741,#7742,#7743,#7744,
#7745,#7746,#7747,#7748),.UNSPECIFIED.,.F.,.F.,(4,2,2,2,4),(0.452348616592526,
0.490044270488251,0.527739924383976,0.565435706587006,0.603131488790035),
 .UNSPECIFIED.);
#275=B_SPLINE_CURVE_WITH_KNOTS('',3,(#7752,#7753,#7754,#7755,#7756,#7757,
#7758,#7759,#7760,#7761),.UNSPECIFIED.,.F.,.F.,(4,2,2,2,4),(0.,0.0376957822030297,
0.0753915644060594,0.113087218301784,0.150782872197509),.UNSPECIFIED.);
#276=B_SPLINE_CURVE_WITH_KNOTS('',3,(#7762,#7763,#7764,#7765,#7766,#7767,
#7768,#7769,#7770,#7771,#7772,#7773,#7774,#7775,#7776,#7777,#7778,#7779,
#7780,#7781,#7782,#7783,#7784,#7785,#7786,#7787),.UNSPECIFIED.,.F.,.F.,
(4,2,2,2,2,2,2,2,2,2,2,2,4),(0.150782872197509,0.188478526093234,0.226174179988958,
0.263869962191988,0.301565744395018,0.339261526598047,0.376957308801077,
0.414652962696802,0.452348616592527,0.490044270488251,0.527739924383976,
0.565435706587006,0.603131488790035),.UNSPECIFIED.);
#277=B_SPLINE_CURVE_WITH_KNOTS('',3,(#7791,#7792,#7793,#7794,#7795,#7796,
#7797,#7798,#7799,#7800,#7801,#7802,#7803,#7804,#7805,#7806,#7807,#7808,
#7809,#7810,#7811,#7812,#7813,#7814,#7815,#7816),.UNSPECIFIED.,.F.,.F.,
(4,2,2,2,2,2,2,2,2,2,2,2,4),(0.,0.0376910486946462,0.0753820973892923,0.113073058602025,
0.150764019814758,0.188454981027491,0.226145942240223,0.26383699093487,
0.301528039629516,0.339219088324161,0.376910137018807,0.41460109823154,
0.452292059444273),.UNSPECIFIED.);
#278=B_SPLINE_CURVE_WITH_KNOTS('',3,(#7817,#7818,#7819,#7820,#7821,#7822,
#7823,#7824,#7825,#7826),.UNSPECIFIED.,.F.,.F.,(4,2,2,2,4),(0.452292059444273,
0.489983020657006,0.527673981869739,0.565365030564385,0.603056079259031),
 .UNSPECIFIED.);
#279=B_SPLINE_CURVE_WITH_KNOTS('',3,(#7830,#7831,#7832,#7833,#7834,#7835,
#7836,#7837,#7838,#7839),.UNSPECIFIED.,.F.,.F.,(4,2,2,2,4),(0.,0.0376910486946459,
0.0753820973892919,0.113073058602025,0.150764019814758),.UNSPECIFIED.);
#280=B_SPLINE_CURVE_WITH_KNOTS('',3,(#7841,#7842,#7843,#7844,#7845,#7846,
#7847,#7848,#7849,#7850),.UNSPECIFIED.,.F.,.F.,(4,2,2,2,4),(0.452292059444274,
0.489983020657007,0.52767398186974,0.565365030564387,0.603056079259033),
 .UNSPECIFIED.);
#281=B_SPLINE_CURVE_WITH_KNOTS('',3,(#7851,#7852,#7853,#7854,#7855,#7856,
#7857,#7858,#7859,#7860,#7861,#7862,#7863,#7864,#7865,#7866,#7867,#7868),
 .UNSPECIFIED.,.F.,.F.,(4,2,2,2,2,2,2,2,4),(0.150764019814758,0.188454981027491,
0.226145942240224,0.26383699093487,0.301528039629516,0.339219088324162,
0.376910137018808,0.414601098231541,0.452292059444274),.UNSPECIFIED.);
#282=B_SPLINE_CURVE_WITH_KNOTS('',3,(#7872,#7873,#7874,#7875,#7876,#7877,
#7878,#7879,#7880,#7881,#7882,#7883,#7884,#7885,#7886,#7887,#7888,#7889),
 .UNSPECIFIED.,.F.,.F.,(4,2,2,2,2,2,2,2,4),(0.15078287219751,0.188478526093235,
0.22617417998896,0.26386996219199,0.301565744395019,0.339261526598049,0.376957308801079,
0.414652962696804,0.452348616592528),.UNSPECIFIED.);
#283=B_SPLINE_CURVE_WITH_KNOTS('',3,(#7891,#7892,#7893,#7894,#7895,#7896,
#7897,#7898,#7899,#7900),.UNSPECIFIED.,.F.,.F.,(4,2,2,2,4),(0.,0.0376957822030297,
0.0753915644060594,0.113087218301785,0.15078287219751),.UNSPECIFIED.);
#284=B_SPLINE_CURVE_WITH_KNOTS('',3,(#7901,#7902,#7903,#7904,#7905,#7906,
#7907,#7908,#7909,#7910),.UNSPECIFIED.,.F.,.F.,(4,2,2,2,4),(0.452348616592528,
0.490044270488253,0.527739924383978,0.565435706587007,0.603131488790037),
 .UNSPECIFIED.);
#285=B_SPLINE_CURVE_WITH_KNOTS('',3,(#7914,#7915,#7916,#7917,#7918,#7919,
#7920,#7921,#7922,#7923),.UNSPECIFIED.,.F.,.F.,(4,2,2,2,4),(0.,0.0376957822030298,
0.0753915644060595,0.113087218301784,0.150782872197509),.UNSPECIFIED.);
#286=B_SPLINE_CURVE_WITH_KNOTS('',3,(#7924,#7925,#7926,#7927,#7928,#7929,
#7930,#7931,#7932,#7933,#7934,#7935,#7936,#7937,#7938,#7939,#7940,#7941,
#7942,#7943,#7944,#7945,#7946,#7947,#7948,#7949),.UNSPECIFIED.,.F.,.F.,
(4,2,2,2,2,2,2,2,2,2,2,2,4),(0.150782872197509,0.188478526093234,0.226174179988959,
0.263869962191988,0.301565744395018,0.339261526598048,0.376957308801077,
0.414652962696803,0.452348616592528,0.490044270488253,0.527739924383978,
0.565435706587008,0.603131488790037),.UNSPECIFIED.);
#287=B_SPLINE_CURVE_WITH_KNOTS('',3,(#7953,#7954,#7955,#7956,#7957,#7958,
#7959,#7960,#7961,#7962,#7963,#7964,#7965,#7966,#7967,#7968,#7969,#7970,
#7971,#7972,#7973,#7974,#7975,#7976,#7977,#7978),.UNSPECIFIED.,.F.,.F.,
(4,2,2,2,2,2,2,2,2,2,2,2,4),(0.,0.0376910486946464,0.0753820973892928,0.113073058602026,
0.150764019814759,0.188454981027492,0.226145942240225,0.263836990934871,
0.301528039629517,0.339219088324163,0.376910137018809,0.414601098231542,
0.452292059444275),.UNSPECIFIED.);
#288=B_SPLINE_CURVE_WITH_KNOTS('',3,(#7979,#7980,#7981,#7982,#7983,#7984,
#7985,#7986,#7987,#7988),.UNSPECIFIED.,.F.,.F.,(4,2,2,2,4),(0.452292059444275,
0.489983020657008,0.527673981869741,0.565365030564387,0.603056079259033),
 .UNSPECIFIED.);
#289=B_SPLINE_CURVE_WITH_KNOTS('',3,(#7992,#7993,#7994,#7995,#7996,#7997,
#7998,#7999,#8000,#8001),.UNSPECIFIED.,.F.,.F.,(4,2,2,2,4),(0.,0.0376910486946462,
0.0753820973892923,0.113073058602025,0.150764019814758),.UNSPECIFIED.);
#290=B_SPLINE_CURVE_WITH_KNOTS('',3,(#8003,#8004,#8005,#8006,#8007,#8008,
#8009,#8010,#8011,#8012),.UNSPECIFIED.,.F.,.F.,(4,2,2,2,4),(0.452292059444276,
0.489983020657008,0.527673981869741,0.565365030564388,0.603056079259034),
 .UNSPECIFIED.);
#291=B_SPLINE_CURVE_WITH_KNOTS('',3,(#8013,#8014,#8015,#8016,#8017,#8018,
#8019,#8020,#8021,#8022,#8023,#8024,#8025,#8026,#8027,#8028,#8029,#8030),
 .UNSPECIFIED.,.F.,.F.,(4,2,2,2,2,2,2,2,4),(0.150764019814758,0.188454981027491,
0.226145942240224,0.263836990934871,0.301528039629517,0.339219088324163,
0.376910137018809,0.414601098231543,0.452292059444276),.UNSPECIFIED.);
#292=B_SPLINE_CURVE_WITH_KNOTS('',3,(#8034,#8035,#8036,#8037,#8038,#8039,
#8040,#8041,#8042,#8043,#8044,#8045,#8046,#8047,#8048,#8049,#8050,#8051),
 .UNSPECIFIED.,.F.,.F.,(4,2,2,2,2,2,2,2,4),(0.150782872197509,0.188478526093234,
0.226174179988959,0.263869962191989,0.301565744395019,0.339261526598048,
0.376957308801078,0.414652962696803,0.452348616592528),.UNSPECIFIED.);
#293=B_SPLINE_CURVE_WITH_KNOTS('',3,(#8053,#8054,#8055,#8056,#8057,#8058,
#8059,#8060,#8061,#8062),.UNSPECIFIED.,.F.,.F.,(4,2,2,2,4),(0.,0.0376957822030297,
0.0753915644060595,0.113087218301784,0.150782872197509),.UNSPECIFIED.);
#294=B_SPLINE_CURVE_WITH_KNOTS('',3,(#8063,#8064,#8065,#8066,#8067,#8068,
#8069,#8070,#8071,#8072),.UNSPECIFIED.,.F.,.F.,(4,2,2,2,4),(0.452348616592528,
0.490044270488253,0.527739924383978,0.565435706587008,0.603131488790038),
 .UNSPECIFIED.);
#295=B_SPLINE_CURVE_WITH_KNOTS('',3,(#8076,#8077,#8078,#8079,#8080,#8081,
#8082,#8083,#8084,#8085),.UNSPECIFIED.,.F.,.F.,(4,2,2,2,4),(0.,0.03769578220303,
0.0753915644060599,0.113087218301785,0.15078287219751),.UNSPECIFIED.);
#296=B_SPLINE_CURVE_WITH_KNOTS('',3,(#8086,#8087,#8088,#8089,#8090,#8091,
#8092,#8093,#8094,#8095,#8096,#8097,#8098,#8099,#8100,#8101,#8102,#8103,
#8104,#8105,#8106,#8107,#8108,#8109,#8110,#8111),.UNSPECIFIED.,.F.,.F.,
(4,2,2,2,2,2,2,2,2,2,2,2,4),(0.15078287219751,0.188478526093235,0.226174179988959,
0.263869962191989,0.301565744395019,0.339261526598049,0.376957308801078,
0.414652962696803,0.452348616592528,0.490044270488253,0.527739924383978,
0.565435706587008,0.603131488790038),.UNSPECIFIED.);
#297=B_SPLINE_CURVE_WITH_KNOTS('',3,(#8115,#8116,#8117,#8118,#8119,#8120,
#8121,#8122,#8123,#8124,#8125,#8126,#8127,#8128,#8129,#8130,#8131,#8132,
#8133,#8134,#8135,#8136,#8137,#8138,#8139,#8140),.UNSPECIFIED.,.F.,.F.,
(4,2,2,2,2,2,2,2,2,2,2,2,4),(0.,0.0376910486946464,0.0753820973892928,0.113073058602026,
0.150764019814759,0.188454981027492,0.226145942240225,0.263836990934871,
0.301528039629517,0.339219088324164,0.37691013701881,0.414601098231543,
0.452292059444276),.UNSPECIFIED.);
#298=B_SPLINE_CURVE_WITH_KNOTS('',3,(#8141,#8142,#8143,#8144,#8145,#8146,
#8147,#8148,#8149,#8150),.UNSPECIFIED.,.F.,.F.,(4,2,2,2,4),(0.452292059444276,
0.489983020657009,0.527673981869742,0.565365030564388,0.603056079259034),
 .UNSPECIFIED.);
#299=B_SPLINE_CURVE_WITH_KNOTS('',3,(#8154,#8155,#8156,#8157,#8158,#8159,
#8160,#8161,#8162,#8163),.UNSPECIFIED.,.F.,.F.,(4,2,2,2,4),(0.,0.0376910486946463,
0.0753820973892926,0.113073058602026,0.150764019814759),.UNSPECIFIED.);
#300=B_SPLINE_CURVE_WITH_KNOTS('',3,(#8165,#8166,#8167,#8168,#8169,#8170,
#8171,#8172,#8173,#8174),.UNSPECIFIED.,.F.,.F.,(4,2,2,2,4),(0.452292059444275,
0.489983020657008,0.527673981869741,0.565365030564388,0.603056079259034),
 .UNSPECIFIED.);
#301=B_SPLINE_CURVE_WITH_KNOTS('',3,(#8175,#8176,#8177,#8178,#8179,#8180,
#8181,#8182,#8183,#8184,#8185,#8186,#8187,#8188,#8189,#8190,#8191,#8192),
 .UNSPECIFIED.,.F.,.F.,(4,2,2,2,2,2,2,2,4),(0.150764019814759,0.188454981027491,
0.226145942240224,0.263836990934871,0.301528039629517,0.339219088324163,
0.37691013701881,0.414601098231543,0.452292059444275),.UNSPECIFIED.);
#302=B_SPLINE_CURVE_WITH_KNOTS('',3,(#8196,#8197,#8198,#8199,#8200,#8201,
#8202,#8203,#8204,#8205,#8206,#8207,#8208,#8209,#8210,#8211,#8212,#8213),
 .UNSPECIFIED.,.F.,.F.,(4,2,2,2,2,2,2,2,4),(0.150782872197509,0.188478526093234,
0.226174179988959,0.263869962191989,0.301565744395019,0.339261526598049,
0.376957308801079,0.414652962696803,0.452348616592528),.UNSPECIFIED.);
#303=B_SPLINE_CURVE_WITH_KNOTS('',3,(#8215,#8216,#8217,#8218,#8219,#8220,
#8221,#8222,#8223,#8224),.UNSPECIFIED.,.F.,.F.,(4,2,2,2,4),(0.,0.0376957822030298,
0.0753915644060597,0.113087218301785,0.150782872197509),.UNSPECIFIED.);
#304=B_SPLINE_CURVE_WITH_KNOTS('',3,(#8225,#8226,#8227,#8228,#8229,#8230,
#8231,#8232,#8233,#8234),.UNSPECIFIED.,.F.,.F.,(4,2,2,2,4),(0.452348616592528,
0.490044270488253,0.527739924383978,0.565435706587008,0.603131488790038),
 .UNSPECIFIED.);
#305=B_SPLINE_CURVE_WITH_KNOTS('',3,(#8238,#8239,#8240,#8241,#8242,#8243,
#8244,#8245,#8246,#8247),.UNSPECIFIED.,.F.,.F.,(4,2,2,2,4),(0.,0.0376957822030298,
0.0753915644060597,0.113087218301785,0.150782872197509),.UNSPECIFIED.);
#306=B_SPLINE_CURVE_WITH_KNOTS('',3,(#8248,#8249,#8250,#8251,#8252,#8253,
#8254,#8255,#8256,#8257,#8258,#8259,#8260,#8261,#8262,#8263,#8264,#8265,
#8266,#8267,#8268,#8269,#8270,#8271,#8272,#8273),.UNSPECIFIED.,.F.,.F.,
(4,2,2,2,2,2,2,2,2,2,2,2,4),(0.150782872197509,0.188478526093234,0.226174179988959,
0.263869962191989,0.301565744395019,0.339261526598049,0.376957308801079,
0.414652962696804,0.452348616592528,0.490044270488253,0.527739924383978,
0.565435706587008,0.603131488790038),.UNSPECIFIED.);
#307=B_SPLINE_CURVE_WITH_KNOTS('',3,(#8277,#8278,#8279,#8280,#8281,#8282,
#8283,#8284,#8285,#8286,#8287,#8288,#8289,#8290,#8291,#8292,#8293,#8294,
#8295,#8296,#8297,#8298,#8299,#8300,#8301,#8302),.UNSPECIFIED.,.F.,.F.,
(4,2,2,2,2,2,2,2,2,2,2,2,4),(0.,0.0376910486946463,0.0753820973892926,0.113073058602026,
0.150764019814759,0.188454981027491,0.226145942240224,0.263836990934871,
0.301528039629517,0.339219088324163,0.37691013701881,0.414601098231543,
0.452292059444275),.UNSPECIFIED.);
#308=B_SPLINE_CURVE_WITH_KNOTS('',3,(#8303,#8304,#8305,#8306,#8307,#8308,
#8309,#8310,#8311,#8312),.UNSPECIFIED.,.F.,.F.,(4,2,2,2,4),(0.452292059444275,
0.489983020657008,0.527673981869741,0.565365030564388,0.603056079259034),
 .UNSPECIFIED.);
#309=B_SPLINE_CURVE_WITH_KNOTS('',3,(#8316,#8317,#8318,#8319,#8320,#8321,
#8322,#8323,#8324,#8325),.UNSPECIFIED.,.F.,.F.,(4,2,2,2,4),(0.,0.0376910486946462,
0.0753820973892923,0.113073058602025,0.150764019814758),.UNSPECIFIED.);
#310=B_SPLINE_CURVE_WITH_KNOTS('',3,(#8327,#8328,#8329,#8330,#8331,#8332,
#8333,#8334,#8335,#8336),.UNSPECIFIED.,.F.,.F.,(4,2,2,2,4),(0.452292059444274,
0.489983020657006,0.527673981869739,0.565365030564385,0.603056079259032),
 .UNSPECIFIED.);
#311=B_SPLINE_CURVE_WITH_KNOTS('',3,(#8337,#8338,#8339,#8340,#8341,#8342,
#8343,#8344,#8345,#8346,#8347,#8348,#8349,#8350,#8351,#8352,#8353,#8354),
 .UNSPECIFIED.,.F.,.F.,(4,2,2,2,2,2,2,2,4),(0.150764019814758,0.188454981027491,
0.226145942240223,0.26383699093487,0.301528039629516,0.339219088324162,
0.376910137018808,0.414601098231541,0.452292059444274),.UNSPECIFIED.);
#312=B_SPLINE_CURVE_WITH_KNOTS('',3,(#8358,#8359,#8360,#8361,#8362,#8363,
#8364,#8365,#8366,#8367,#8368,#8369,#8370,#8371,#8372,#8373,#8374,#8375),
 .UNSPECIFIED.,.F.,.F.,(4,2,2,2,2,2,2,2,4),(0.150782872197509,0.188478526093234,
0.226174179988958,0.263869962191988,0.301565744395018,0.339261526598047,
0.376957308801077,0.414652962696802,0.452348616592526),.UNSPECIFIED.);
#313=B_SPLINE_CURVE_WITH_KNOTS('',3,(#8377,#8378,#8379,#8380,#8381,#8382,
#8383,#8384,#8385,#8386),.UNSPECIFIED.,.F.,.F.,(4,2,2,2,4),(0.,0.0376957822030297,
0.0753915644060594,0.113087218301784,0.150782872197509),.UNSPECIFIED.);
#314=B_SPLINE_CURVE_WITH_KNOTS('',3,(#8387,#8388,#8389,#8390,#8391,#8392,
#8393,#8394,#8395,#8396),.UNSPECIFIED.,.F.,.F.,(4,2,2,2,4),(0.452348616592526,
0.490044270488251,0.527739924383976,0.565435706587006,0.603131488790035),
 .UNSPECIFIED.);
#315=B_SPLINE_CURVE_WITH_KNOTS('',3,(#8400,#8401,#8402,#8403,#8404,#8405,
#8406,#8407,#8408,#8409),.UNSPECIFIED.,.F.,.F.,(4,2,2,2,4),(0.,0.0376957822030297,
0.0753915644060594,0.113087218301784,0.150782872197509),.UNSPECIFIED.);
#316=B_SPLINE_CURVE_WITH_KNOTS('',3,(#8410,#8411,#8412,#8413,#8414,#8415,
#8416,#8417,#8418,#8419,#8420,#8421,#8422,#8423,#8424,#8425,#8426,#8427,
#8428,#8429,#8430,#8431,#8432,#8433,#8434,#8435),.UNSPECIFIED.,.F.,.F.,
(4,2,2,2,2,2,2,2,2,2,2,2,4),(0.150782872197509,0.188478526093234,0.226174179988958,
0.263869962191988,0.301565744395018,0.339261526598047,0.376957308801077,
0.414652962696802,0.452348616592527,0.490044270488251,0.527739924383976,
0.565435706587006,0.603131488790035),.UNSPECIFIED.);
#317=B_SPLINE_CURVE_WITH_KNOTS('',3,(#8439,#8440,#8441,#8442,#8443,#8444,
#8445,#8446,#8447,#8448,#8449,#8450,#8451,#8452,#8453,#8454,#8455,#8456,
#8457,#8458,#8459,#8460,#8461,#8462,#8463,#8464),.UNSPECIFIED.,.F.,.F.,
(4,2,2,2,2,2,2,2,2,2,2,2,4),(0.,0.0376910486946462,0.0753820973892923,0.113073058602025,
0.150764019814758,0.188454981027491,0.226145942240223,0.26383699093487,
0.301528039629516,0.339219088324162,0.376910137018808,0.414601098231541,
0.452292059444274),.UNSPECIFIED.);
#318=B_SPLINE_CURVE_WITH_KNOTS('',3,(#8465,#8466,#8467,#8468,#8469,#8470,
#8471,#8472,#8473,#8474),.UNSPECIFIED.,.F.,.F.,(4,2,2,2,4),(0.452292059444274,
0.489983020657006,0.527673981869739,0.565365030564385,0.603056079259032),
 .UNSPECIFIED.);
#319=FACE_BOUND('',#677,.T.);
#320=FACE_BOUND('',#687,.T.);
#321=FACE_BOUND('',#690,.T.);
#322=FACE_BOUND('',#693,.T.);
#323=FACE_BOUND('',#694,.T.);
#324=FACE_BOUND('',#695,.T.);
#325=FACE_BOUND('',#696,.T.);
#326=FACE_BOUND('',#697,.T.);
#327=FACE_BOUND('',#701,.T.);
#328=FACE_BOUND('',#702,.T.);
#329=FACE_BOUND('',#703,.T.);
#330=FACE_BOUND('',#704,.T.);
#331=FACE_BOUND('',#705,.T.);
#332=FACE_BOUND('',#707,.T.);
#333=FACE_BOUND('',#709,.T.);
#334=FACE_BOUND('',#711,.T.);
#335=FACE_BOUND('',#762,.T.);
#336=FACE_BOUND('',#763,.T.);
#337=FACE_BOUND('',#764,.T.);
#338=FACE_BOUND('',#765,.T.);
#339=FACE_BOUND('',#766,.T.);
#340=FACE_BOUND('',#767,.T.);
#341=FACE_BOUND('',#768,.T.);
#342=FACE_BOUND('',#769,.T.);
#343=FACE_BOUND('',#770,.T.);
#344=FACE_BOUND('',#771,.T.);
#345=FACE_BOUND('',#772,.T.);
#346=FACE_BOUND('',#773,.T.);
#347=FACE_BOUND('',#774,.T.);
#348=FACE_BOUND('',#775,.T.);
#349=FACE_BOUND('',#776,.T.);
#350=FACE_BOUND('',#777,.T.);
#351=FACE_BOUND('',#778,.T.);
#352=FACE_BOUND('',#779,.T.);
#353=FACE_BOUND('',#780,.T.);
#354=FACE_BOUND('',#781,.T.);
#355=FACE_BOUND('',#782,.T.);
#356=FACE_BOUND('',#783,.T.);
#357=FACE_BOUND('',#784,.T.);
#358=FACE_BOUND('',#785,.T.);
#359=FACE_BOUND('',#786,.T.);
#360=FACE_BOUND('',#787,.T.);
#361=FACE_BOUND('',#788,.T.);
#362=FACE_BOUND('',#789,.T.);
#363=FACE_BOUND('',#790,.T.);
#364=FACE_BOUND('',#791,.T.);
#365=FACE_BOUND('',#792,.T.);
#366=FACE_BOUND('',#793,.T.);
#367=FACE_BOUND('',#794,.T.);
#368=FACE_BOUND('',#795,.T.);
#369=FACE_BOUND('',#796,.T.);
#370=FACE_BOUND('',#797,.T.);
#371=FACE_BOUND('',#798,.T.);
#372=FACE_BOUND('',#799,.T.);
#373=FACE_BOUND('',#800,.T.);
#374=FACE_BOUND('',#801,.T.);
#375=FACE_BOUND('',#802,.T.);
#376=FACE_BOUND('',#803,.T.);
#377=FACE_BOUND('',#805,.T.);
#378=FACE_BOUND('',#807,.T.);
#379=FACE_BOUND('',#810,.T.);
#380=FACE_BOUND('',#811,.T.);
#381=FACE_BOUND('',#812,.T.);
#382=FACE_BOUND('',#813,.T.);
#383=FACE_BOUND('',#814,.T.);
#384=FACE_BOUND('',#815,.T.);
#385=FACE_BOUND('',#816,.T.);
#386=FACE_BOUND('',#817,.T.);
#387=FACE_BOUND('',#818,.T.);
#388=FACE_BOUND('',#819,.T.);
#389=FACE_BOUND('',#820,.T.);
#390=FACE_BOUND('',#821,.T.);
#391=FACE_BOUND('',#822,.T.);
#392=FACE_BOUND('',#823,.T.);
#393=FACE_BOUND('',#824,.T.);
#394=FACE_BOUND('',#825,.T.);
#395=FACE_BOUND('',#826,.T.);
#396=FACE_BOUND('',#827,.T.);
#397=FACE_BOUND('',#828,.T.);
#398=FACE_BOUND('',#829,.T.);
#399=FACE_BOUND('',#830,.T.);
#400=FACE_BOUND('',#831,.T.);
#401=FACE_BOUND('',#832,.T.);
#402=FACE_BOUND('',#833,.T.);
#403=FACE_BOUND('',#834,.T.);
#404=FACE_BOUND('',#835,.T.);
#405=FACE_BOUND('',#836,.T.);
#406=FACE_BOUND('',#837,.T.);
#407=FACE_BOUND('',#838,.T.);
#408=FACE_BOUND('',#839,.T.);
#409=FACE_BOUND('',#840,.T.);
#410=FACE_BOUND('',#841,.T.);
#411=FACE_BOUND('',#842,.T.);
#412=FACE_BOUND('',#843,.T.);
#413=FACE_BOUND('',#844,.T.);
#414=FACE_BOUND('',#845,.T.);
#415=FACE_BOUND('',#846,.T.);
#416=FACE_BOUND('',#847,.T.);
#417=FACE_BOUND('',#848,.T.);
#418=FACE_BOUND('',#849,.T.);
#419=FACE_BOUND('',#850,.T.);
#420=FACE_BOUND('',#851,.T.);
#421=FACE_BOUND('',#853,.T.);
#422=FACE_BOUND('',#855,.T.);
#423=FACE_BOUND('',#859,.T.);
#424=FACE_BOUND('',#861,.T.);
#425=FACE_BOUND('',#865,.T.);
#426=FACE_BOUND('',#867,.T.);
#427=FACE_BOUND('',#871,.T.);
#428=FACE_BOUND('',#873,.T.);
#429=FACE_BOUND('',#881,.T.);
#430=FACE_BOUND('',#882,.T.);
#431=FACE_BOUND('',#883,.T.);
#432=FACE_BOUND('',#884,.T.);
#433=FACE_BOUND('',#885,.T.);
#434=FACE_BOUND('',#887,.T.);
#435=FACE_BOUND('',#888,.T.);
#436=FACE_BOUND('',#889,.T.);
#437=FACE_BOUND('',#890,.T.);
#438=FACE_BOUND('',#891,.T.);
#439=FACE_BOUND('',#899,.T.);
#440=FACE_BOUND('',#902,.T.);
#441=FACE_BOUND('',#903,.T.);
#442=FACE_BOUND('',#904,.T.);
#443=FACE_BOUND('',#905,.T.);
#444=FACE_BOUND('',#906,.T.);
#445=FACE_BOUND('',#908,.T.);
#446=FACE_BOUND('',#909,.T.);
#447=FACE_BOUND('',#910,.T.);
#448=FACE_BOUND('',#911,.T.);
#449=FACE_BOUND('',#912,.T.);
#450=FACE_BOUND('',#918,.T.);
#451=FACE_BOUND('',#932,.T.);
#452=FACE_BOUND('',#934,.T.);
#453=FACE_BOUND('',#943,.T.);
#454=FACE_BOUND('',#948,.T.);
#455=FACE_BOUND('',#951,.T.);
#456=ELLIPSE('',#3509,1.11722871427475,0.79);
#457=ELLIPSE('',#3511,1.11722871427475,0.79);
#458=ELLIPSE('',#3522,1.11722871427475,0.79);
#459=ELLIPSE('',#3524,1.11722871427475,0.79);
#460=ELLIPSE('',#3527,1.11722871427475,0.79);
#461=ELLIPSE('',#3528,1.11722871427475,0.79);
#462=ELLIPSE('',#3548,5.22625185950551,2.);
#463=ELLIPSE('',#3549,2.16478440058479,2.);
#464=ELLIPSE('',#3550,5.22625185950551,2.);
#465=PLANE('',#3508);
#466=PLANE('',#3515);
#467=PLANE('',#3521);
#468=PLANE('',#3529);
#469=PLANE('',#3535);
#470=PLANE('',#3540);
#471=PLANE('',#3542);
#472=PLANE('',#3551);
#473=PLANE('',#3555);
#474=PLANE('',#3556);
#475=PLANE('',#3612);
#476=PLANE('',#3613);
#477=PLANE('',#3620);
#478=PLANE('',#3621);
#479=PLANE('',#3628);
#480=PLANE('',#3629);
#481=PLANE('',#3637);
#482=PLANE('',#3638);
#483=PLANE('',#3646);
#484=PLANE('',#3647);
#485=PLANE('',#3667);
#486=PLANE('',#3668);
#487=PLANE('',#3688);
#488=PLANE('',#3692);
#489=PLANE('',#3693);
#490=PLANE('',#3695);
#491=PLANE('',#3703);
#492=PLANE('',#3711);
#493=PLANE('',#3712);
#494=PLANE('',#3713);
#495=PLANE('',#3714);
#496=PLANE('',#3715);
#497=PLANE('',#3716);
#498=PLANE('',#3717);
#499=PLANE('',#3718);
#500=PLANE('',#3719);
#501=PLANE('',#3721);
#502=PLANE('',#3723);
#503=PLANE('',#3725);
#504=PLANE('',#3726);
#505=PLANE('',#3727);
#506=PLANE('',#3728);
#507=PLANE('',#3729);
#508=PLANE('',#3730);
#509=PLANE('',#3733);
#510=PLANE('',#3741);
#511=PLANE('',#3745);
#512=PLANE('',#3747);
#513=PLANE('',#3748);
#514=PLANE('',#3749);
#515=PLANE('',#3750);
#516=PLANE('',#3751);
#517=PLANE('',#3752);
#518=PLANE('',#3753);
#519=PLANE('',#3756);
#520=FACE_OUTER_BOUND('',#672,.T.);
#521=FACE_OUTER_BOUND('',#673,.T.);
#522=FACE_OUTER_BOUND('',#674,.T.);
#523=FACE_OUTER_BOUND('',#675,.T.);
#524=FACE_OUTER_BOUND('',#676,.T.);
#525=FACE_OUTER_BOUND('',#678,.T.);
#526=FACE_OUTER_BOUND('',#679,.T.);
#527=FACE_OUTER_BOUND('',#680,.T.);
#528=FACE_OUTER_BOUND('',#681,.T.);
#529=FACE_OUTER_BOUND('',#682,.T.);
#530=FACE_OUTER_BOUND('',#683,.T.);
#531=FACE_OUTER_BOUND('',#684,.T.);
#532=FACE_OUTER_BOUND('',#685,.T.);
#533=FACE_OUTER_BOUND('',#686,.T.);
#534=FACE_OUTER_BOUND('',#688,.T.);
#535=FACE_OUTER_BOUND('',#689,.T.);
#536=FACE_OUTER_BOUND('',#691,.T.);
#537=FACE_OUTER_BOUND('',#692,.T.);
#538=FACE_OUTER_BOUND('',#698,.T.);
#539=FACE_OUTER_BOUND('',#699,.T.);
#540=FACE_OUTER_BOUND('',#700,.T.);
#541=FACE_OUTER_BOUND('',#706,.T.);
#542=FACE_OUTER_BOUND('',#708,.T.);
#543=FACE_OUTER_BOUND('',#710,.T.);
#544=FACE_OUTER_BOUND('',#712,.T.);
#545=FACE_OUTER_BOUND('',#713,.T.);
#546=FACE_OUTER_BOUND('',#714,.T.);
#547=FACE_OUTER_BOUND('',#715,.T.);
#548=FACE_OUTER_BOUND('',#716,.T.);
#549=FACE_OUTER_BOUND('',#717,.T.);
#550=FACE_OUTER_BOUND('',#718,.T.);
#551=FACE_OUTER_BOUND('',#719,.T.);
#552=FACE_OUTER_BOUND('',#720,.T.);
#553=FACE_OUTER_BOUND('',#721,.T.);
#554=FACE_OUTER_BOUND('',#722,.T.);
#555=FACE_OUTER_BOUND('',#723,.T.);
#556=FACE_OUTER_BOUND('',#724,.T.);
#557=FACE_OUTER_BOUND('',#725,.T.);
#558=FACE_OUTER_BOUND('',#726,.T.);
#559=FACE_OUTER_BOUND('',#727,.T.);
#560=FACE_OUTER_BOUND('',#728,.T.);
#561=FACE_OUTER_BOUND('',#729,.T.);
#562=FACE_OUTER_BOUND('',#730,.T.);
#563=FACE_OUTER_BOUND('',#731,.T.);
#564=FACE_OUTER_BOUND('',#732,.T.);
#565=FACE_OUTER_BOUND('',#733,.T.);
#566=FACE_OUTER_BOUND('',#734,.T.);
#567=FACE_OUTER_BOUND('',#735,.T.);
#568=FACE_OUTER_BOUND('',#736,.T.);
#569=FACE_OUTER_BOUND('',#737,.T.);
#570=FACE_OUTER_BOUND('',#738,.T.);
#571=FACE_OUTER_BOUND('',#739,.T.);
#572=FACE_OUTER_BOUND('',#740,.T.);
#573=FACE_OUTER_BOUND('',#741,.T.);
#574=FACE_OUTER_BOUND('',#742,.T.);
#575=FACE_OUTER_BOUND('',#743,.T.);
#576=FACE_OUTER_BOUND('',#744,.T.);
#577=FACE_OUTER_BOUND('',#745,.T.);
#578=FACE_OUTER_BOUND('',#746,.T.);
#579=FACE_OUTER_BOUND('',#747,.T.);
#580=FACE_OUTER_BOUND('',#748,.T.);
#581=FACE_OUTER_BOUND('',#749,.T.);
#582=FACE_OUTER_BOUND('',#750,.T.);
#583=FACE_OUTER_BOUND('',#751,.T.);
#584=FACE_OUTER_BOUND('',#752,.T.);
#585=FACE_OUTER_BOUND('',#753,.T.);
#586=FACE_OUTER_BOUND('',#754,.T.);
#587=FACE_OUTER_BOUND('',#755,.T.);
#588=FACE_OUTER_BOUND('',#756,.T.);
#589=FACE_OUTER_BOUND('',#757,.T.);
#590=FACE_OUTER_BOUND('',#758,.T.);
#591=FACE_OUTER_BOUND('',#759,.T.);
#592=FACE_OUTER_BOUND('',#760,.T.);
#593=FACE_OUTER_BOUND('',#761,.T.);
#594=FACE_OUTER_BOUND('',#804,.T.);
#595=FACE_OUTER_BOUND('',#806,.T.);
#596=FACE_OUTER_BOUND('',#808,.T.);
#597=FACE_OUTER_BOUND('',#809,.T.);
#598=FACE_OUTER_BOUND('',#852,.T.);
#599=FACE_OUTER_BOUND('',#854,.T.);
#600=FACE_OUTER_BOUND('',#856,.T.);
#601=FACE_OUTER_BOUND('',#857,.T.);
#602=FACE_OUTER_BOUND('',#858,.T.);
#603=FACE_OUTER_BOUND('',#860,.T.);
#604=FACE_OUTER_BOUND('',#862,.T.);
#605=FACE_OUTER_BOUND('',#863,.T.);
#606=FACE_OUTER_BOUND('',#864,.T.);
#607=FACE_OUTER_BOUND('',#866,.T.);
#608=FACE_OUTER_BOUND('',#868,.T.);
#609=FACE_OUTER_BOUND('',#869,.T.);
#610=FACE_OUTER_BOUND('',#870,.T.);
#611=FACE_OUTER_BOUND('',#872,.T.);
#612=FACE_OUTER_BOUND('',#874,.T.);
#613=FACE_OUTER_BOUND('',#875,.T.);
#614=FACE_OUTER_BOUND('',#876,.T.);
#615=FACE_OUTER_BOUND('',#877,.T.);
#616=FACE_OUTER_BOUND('',#878,.T.);
#617=FACE_OUTER_BOUND('',#879,.T.);
#618=FACE_OUTER_BOUND('',#880,.T.);
#619=FACE_OUTER_BOUND('',#886,.T.);
#620=FACE_OUTER_BOUND('',#892,.T.);
#621=FACE_OUTER_BOUND('',#893,.T.);
#622=FACE_OUTER_BOUND('',#894,.T.);
#623=FACE_OUTER_BOUND('',#895,.T.);
#624=FACE_OUTER_BOUND('',#896,.T.);
#625=FACE_OUTER_BOUND('',#897,.T.);
#626=FACE_OUTER_BOUND('',#898,.T.);
#627=FACE_OUTER_BOUND('',#900,.T.);
#628=FACE_OUTER_BOUND('',#901,.T.);
#629=FACE_OUTER_BOUND('',#907,.T.);
#630=FACE_OUTER_BOUND('',#913,.T.);
#631=FACE_OUTER_BOUND('',#914,.T.);
#632=FACE_OUTER_BOUND('',#915,.T.);
#633=FACE_OUTER_BOUND('',#916,.T.);
#634=FACE_OUTER_BOUND('',#917,.T.);
#635=FACE_OUTER_BOUND('',#919,.T.);
#636=FACE_OUTER_BOUND('',#920,.T.);
#637=FACE_OUTER_BOUND('',#921,.T.);
#638=FACE_OUTER_BOUND('',#922,.T.);
#639=FACE_OUTER_BOUND('',#923,.T.);
#640=FACE_OUTER_BOUND('',#924,.T.);
#641=FACE_OUTER_BOUND('',#925,.T.);
#642=FACE_OUTER_BOUND('',#926,.T.);
#643=FACE_OUTER_BOUND('',#927,.T.);
#644=FACE_OUTER_BOUND('',#928,.T.);
#645=FACE_OUTER_BOUND('',#929,.T.);
#646=FACE_OUTER_BOUND('',#930,.T.);
#647=FACE_OUTER_BOUND('',#931,.T.);
#648=FACE_OUTER_BOUND('',#933,.T.);
#649=FACE_OUTER_BOUND('',#935,.T.);
#650=FACE_OUTER_BOUND('',#936,.T.);
#651=FACE_OUTER_BOUND('',#937,.T.);
#652=FACE_OUTER_BOUND('',#938,.T.);
#653=FACE_OUTER_BOUND('',#939,.T.);
#654=FACE_OUTER_BOUND('',#940,.T.);
#655=FACE_OUTER_BOUND('',#941,.T.);
#656=FACE_OUTER_BOUND('',#942,.T.);
#657=FACE_OUTER_BOUND('',#944,.T.);
#658=FACE_OUTER_BOUND('',#945,.T.);
#659=FACE_OUTER_BOUND('',#946,.T.);
#660=FACE_OUTER_BOUND('',#947,.T.);
#661=FACE_OUTER_BOUND('',#949,.T.);
#662=FACE_OUTER_BOUND('',#950,.T.);
#663=FACE_OUTER_BOUND('',#952,.T.);
#664=FACE_OUTER_BOUND('',#953,.T.);
#665=FACE_OUTER_BOUND('',#954,.T.);
#666=FACE_OUTER_BOUND('',#955,.T.);
#667=FACE_OUTER_BOUND('',#956,.T.);
#668=FACE_OUTER_BOUND('',#957,.T.);
#669=FACE_OUTER_BOUND('',#958,.T.);
#670=FACE_OUTER_BOUND('',#959,.T.);
#671=FACE_OUTER_BOUND('',#960,.T.);
#672=EDGE_LOOP('',(#2194,#2195,#2196,#2197));
#673=EDGE_LOOP('',(#2198,#2199,#2200,#2201));
#674=EDGE_LOOP('',(#2202,#2203,#2204,#2205));
#675=EDGE_LOOP('',(#2206,#2207,#2208,#2209));
#676=EDGE_LOOP('',(#2210,#2211,#2212,#2213));
#677=EDGE_LOOP('',(#2214));
#678=EDGE_LOOP('',(#2215,#2216,#2217,#2218,#2219,#2220));
#679=EDGE_LOOP('',(#2221,#2222,#2223));
#680=EDGE_LOOP('',(#2224,#2225,#2226,#2227,#2228,#2229));
#681=EDGE_LOOP('',(#2230,#2231,#2232,#2233,#2234));
#682=EDGE_LOOP('',(#2235,#2236,#2237,#2238,#2239,#2240,#2241,#2242,#2243,
#2244));
#683=EDGE_LOOP('',(#2245,#2246,#2247));
#684=EDGE_LOOP('',(#2248,#2249,#2250,#2251));
#685=EDGE_LOOP('',(#2252,#2253,#2254,#2255));
#686=EDGE_LOOP('',(#2256));
#687=EDGE_LOOP('',(#2257));
#688=EDGE_LOOP('',(#2258,#2259,#2260,#2261));
#689=EDGE_LOOP('',(#2262));
#690=EDGE_LOOP('',(#2263));
#691=EDGE_LOOP('',(#2264,#2265,#2266,#2267,#2268,#2269,#2270,#2271,#2272));
#692=EDGE_LOOP('',(#2273));
#693=EDGE_LOOP('',(#2274));
#694=EDGE_LOOP('',(#2275));
#695=EDGE_LOOP('',(#2276));
#696=EDGE_LOOP('',(#2277));
#697=EDGE_LOOP('',(#2278));
#698=EDGE_LOOP('',(#2279,#2280,#2281,#2282));
#699=EDGE_LOOP('',(#2283,#2284,#2285,#2286,#2287,#2288));
#700=EDGE_LOOP('',(#2289));
#701=EDGE_LOOP('',(#2290));
#702=EDGE_LOOP('',(#2291));
#703=EDGE_LOOP('',(#2292));
#704=EDGE_LOOP('',(#2293));
#705=EDGE_LOOP('',(#2294));
#706=EDGE_LOOP('',(#2295,#2296,#2297,#2298));
#707=EDGE_LOOP('',(#2299,#2300,#2301));
#708=EDGE_LOOP('',(#2302));
#709=EDGE_LOOP('',(#2303));
#710=EDGE_LOOP('',(#2304));
#711=EDGE_LOOP('',(#2305));
#712=EDGE_LOOP('',(#2306,#2307,#2308,#2309,#2310,#2311));
#713=EDGE_LOOP('',(#2312,#2313,#2314,#2315,#2316,#2317));
#714=EDGE_LOOP('',(#2318,#2319,#2320,#2321,#2322,#2323));
#715=EDGE_LOOP('',(#2324,#2325,#2326,#2327,#2328,#2329));
#716=EDGE_LOOP('',(#2330,#2331,#2332,#2333,#2334,#2335));
#717=EDGE_LOOP('',(#2336,#2337,#2338,#2339,#2340,#2341));
#718=EDGE_LOOP('',(#2342,#2343,#2344,#2345,#2346,#2347));
#719=EDGE_LOOP('',(#2348,#2349,#2350,#2351,#2352,#2353));
#720=EDGE_LOOP('',(#2354,#2355,#2356,#2357,#2358,#2359));
#721=EDGE_LOOP('',(#2360,#2361,#2362,#2363,#2364,#2365));
#722=EDGE_LOOP('',(#2366,#2367,#2368,#2369,#2370,#2371));
#723=EDGE_LOOP('',(#2372,#2373,#2374,#2375,#2376,#2377));
#724=EDGE_LOOP('',(#2378,#2379,#2380,#2381,#2382,#2383));
#725=EDGE_LOOP('',(#2384,#2385,#2386,#2387,#2388,#2389));
#726=EDGE_LOOP('',(#2390,#2391,#2392,#2393,#2394,#2395));
#727=EDGE_LOOP('',(#2396,#2397,#2398,#2399,#2400,#2401));
#728=EDGE_LOOP('',(#2402,#2403,#2404,#2405,#2406,#2407));
#729=EDGE_LOOP('',(#2408,#2409,#2410,#2411,#2412,#2413));
#730=EDGE_LOOP('',(#2414,#2415,#2416,#2417,#2418,#2419));
#731=EDGE_LOOP('',(#2420,#2421,#2422,#2423,#2424,#2425));
#732=EDGE_LOOP('',(#2426,#2427,#2428,#2429,#2430,#2431));
#733=EDGE_LOOP('',(#2432,#2433,#2434,#2435,#2436,#2437));
#734=EDGE_LOOP('',(#2438,#2439,#2440,#2441,#2442,#2443));
#735=EDGE_LOOP('',(#2444,#2445,#2446,#2447,#2448,#2449));
#736=EDGE_LOOP('',(#2450,#2451,#2452,#2453,#2454,#2455));
#737=EDGE_LOOP('',(#2456,#2457,#2458,#2459,#2460,#2461));
#738=EDGE_LOOP('',(#2462,#2463,#2464,#2465,#2466,#2467));
#739=EDGE_LOOP('',(#2468,#2469,#2470,#2471,#2472,#2473));
#740=EDGE_LOOP('',(#2474,#2475,#2476,#2477,#2478,#2479));
#741=EDGE_LOOP('',(#2480,#2481,#2482,#2483,#2484,#2485));
#742=EDGE_LOOP('',(#2486,#2487,#2488,#2489,#2490,#2491));
#743=EDGE_LOOP('',(#2492,#2493,#2494,#2495,#2496,#2497));
#744=EDGE_LOOP('',(#2498,#2499,#2500,#2501,#2502,#2503));
#745=EDGE_LOOP('',(#2504,#2505,#2506,#2507,#2508,#2509));
#746=EDGE_LOOP('',(#2510,#2511,#2512,#2513,#2514,#2515));
#747=EDGE_LOOP('',(#2516,#2517,#2518,#2519,#2520,#2521));
#748=EDGE_LOOP('',(#2522,#2523,#2524,#2525,#2526,#2527,#2528,#2529));
#749=EDGE_LOOP('',(#2530,#2531,#2532,#2533,#2534,#2535));
#750=EDGE_LOOP('',(#2536,#2537,#2538,#2539,#2540,#2541,#2542,#2543));
#751=EDGE_LOOP('',(#2544,#2545,#2546,#2547,#2548,#2549));
#752=EDGE_LOOP('',(#2550,#2551,#2552,#2553,#2554,#2555,#2556,#2557));
#753=EDGE_LOOP('',(#2558,#2559,#2560,#2561,#2562,#2563));
#754=EDGE_LOOP('',(#2564,#2565,#2566,#2567,#2568,#2569,#2570,#2571));
#755=EDGE_LOOP('',(#2572,#2573,#2574,#2575,#2576,#2577));
#756=EDGE_LOOP('',(#2578,#2579,#2580,#2581,#2582,#2583,#2584,#2585));
#757=EDGE_LOOP('',(#2586,#2587,#2588,#2589,#2590,#2591));
#758=EDGE_LOOP('',(#2592,#2593,#2594,#2595,#2596,#2597,#2598,#2599));
#759=EDGE_LOOP('',(#2600,#2601,#2602,#2603,#2604,#2605));
#760=EDGE_LOOP('',(#2606,#2607,#2608,#2609));
#761=EDGE_LOOP('',(#2610,#2611,#2612,#2613,#2614,#2615,#2616,#2617,#2618,
#2619,#2620,#2621,#2622,#2623,#2624,#2625,#2626,#2627,#2628,#2629,#2630,
#2631,#2632,#2633,#2634,#2635,#2636,#2637,#2638,#2639,#2640,#2641,#2642,
#2643));
#762=EDGE_LOOP('',(#2644,#2645));
#763=EDGE_LOOP('',(#2646,#2647));
#764=EDGE_LOOP('',(#2648,#2649));
#765=EDGE_LOOP('',(#2650,#2651));
#766=EDGE_LOOP('',(#2652,#2653));
#767=EDGE_LOOP('',(#2654,#2655));
#768=EDGE_LOOP('',(#2656,#2657));
#769=EDGE_LOOP('',(#2658,#2659));
#770=EDGE_LOOP('',(#2660,#2661));
#771=EDGE_LOOP('',(#2662,#2663));
#772=EDGE_LOOP('',(#2664,#2665));
#773=EDGE_LOOP('',(#2666,#2667));
#774=EDGE_LOOP('',(#2668,#2669));
#775=EDGE_LOOP('',(#2670,#2671));
#776=EDGE_LOOP('',(#2672,#2673));
#777=EDGE_LOOP('',(#2674,#2675));
#778=EDGE_LOOP('',(#2676,#2677));
#779=EDGE_LOOP('',(#2678,#2679));
#780=EDGE_LOOP('',(#2680,#2681));
#781=EDGE_LOOP('',(#2682,#2683));
#782=EDGE_LOOP('',(#2684,#2685));
#783=EDGE_LOOP('',(#2686,#2687));
#784=EDGE_LOOP('',(#2688,#2689));
#785=EDGE_LOOP('',(#2690,#2691));
#786=EDGE_LOOP('',(#2692,#2693));
#787=EDGE_LOOP('',(#2694,#2695));
#788=EDGE_LOOP('',(#2696,#2697));
#789=EDGE_LOOP('',(#2698,#2699));
#790=EDGE_LOOP('',(#2700,#2701));
#791=EDGE_LOOP('',(#2702,#2703));
#792=EDGE_LOOP('',(#2704,#2705));
#793=EDGE_LOOP('',(#2706,#2707));
#794=EDGE_LOOP('',(#2708,#2709));
#795=EDGE_LOOP('',(#2710,#2711));
#796=EDGE_LOOP('',(#2712,#2713));
#797=EDGE_LOOP('',(#2714,#2715));
#798=EDGE_LOOP('',(#2716,#2717));
#799=EDGE_LOOP('',(#2718,#2719));
#800=EDGE_LOOP('',(#2720,#2721));
#801=EDGE_LOOP('',(#2722,#2723));
#802=EDGE_LOOP('',(#2724,#2725));
#803=EDGE_LOOP('',(#2726,#2727));
#804=EDGE_LOOP('',(#2728));
#805=EDGE_LOOP('',(#2729));
#806=EDGE_LOOP('',(#2730));
#807=EDGE_LOOP('',(#2731));
#808=EDGE_LOOP('',(#2732,#2733,#2734,#2735));
#809=EDGE_LOOP('',(#2736,#2737,#2738,#2739,#2740,#2741,#2742,#2743,#2744,
#2745,#2746,#2747,#2748,#2749,#2750,#2751,#2752,#2753,#2754,#2755,#2756,
#2757,#2758,#2759,#2760,#2761,#2762,#2763,#2764,#2765,#2766,#2767,#2768,
#2769));
#810=EDGE_LOOP('',(#2770,#2771));
#811=EDGE_LOOP('',(#2772,#2773));
#812=EDGE_LOOP('',(#2774,#2775));
#813=EDGE_LOOP('',(#2776,#2777));
#814=EDGE_LOOP('',(#2778,#2779));
#815=EDGE_LOOP('',(#2780,#2781));
#816=EDGE_LOOP('',(#2782,#2783));
#817=EDGE_LOOP('',(#2784,#2785));
#818=EDGE_LOOP('',(#2786,#2787));
#819=EDGE_LOOP('',(#2788,#2789));
#820=EDGE_LOOP('',(#2790,#2791));
#821=EDGE_LOOP('',(#2792,#2793));
#822=EDGE_LOOP('',(#2794,#2795));
#823=EDGE_LOOP('',(#2796,#2797));
#824=EDGE_LOOP('',(#2798,#2799));
#825=EDGE_LOOP('',(#2800,#2801));
#826=EDGE_LOOP('',(#2802,#2803));
#827=EDGE_LOOP('',(#2804,#2805));
#828=EDGE_LOOP('',(#2806,#2807));
#829=EDGE_LOOP('',(#2808,#2809));
#830=EDGE_LOOP('',(#2810,#2811));
#831=EDGE_LOOP('',(#2812,#2813));
#832=EDGE_LOOP('',(#2814,#2815));
#833=EDGE_LOOP('',(#2816,#2817));
#834=EDGE_LOOP('',(#2818,#2819));
#835=EDGE_LOOP('',(#2820,#2821));
#836=EDGE_LOOP('',(#2822,#2823));
#837=EDGE_LOOP('',(#2824,#2825));
#838=EDGE_LOOP('',(#2826,#2827));
#839=EDGE_LOOP('',(#2828,#2829));
#840=EDGE_LOOP('',(#2830,#2831));
#841=EDGE_LOOP('',(#2832,#2833));
#842=EDGE_LOOP('',(#2834,#2835));
#843=EDGE_LOOP('',(#2836,#2837));
#844=EDGE_LOOP('',(#2838,#2839));
#845=EDGE_LOOP('',(#2840,#2841));
#846=EDGE_LOOP('',(#2842,#2843));
#847=EDGE_LOOP('',(#2844,#2845));
#848=EDGE_LOOP('',(#2846,#2847));
#849=EDGE_LOOP('',(#2848,#2849));
#850=EDGE_LOOP('',(#2850,#2851));
#851=EDGE_LOOP('',(#2852,#2853));
#852=EDGE_LOOP('',(#2854));
#853=EDGE_LOOP('',(#2855));
#854=EDGE_LOOP('',(#2856));
#855=EDGE_LOOP('',(#2857));
#856=EDGE_LOOP('',(#2858,#2859,#2860,#2861));
#857=EDGE_LOOP('',(#2862,#2863,#2864,#2865));
#858=EDGE_LOOP('',(#2866));
#859=EDGE_LOOP('',(#2867));
#860=EDGE_LOOP('',(#2868));
#861=EDGE_LOOP('',(#2869));
#862=EDGE_LOOP('',(#2870,#2871,#2872,#2873));
#863=EDGE_LOOP('',(#2874,#2875,#2876,#2877));
#864=EDGE_LOOP('',(#2878));
#865=EDGE_LOOP('',(#2879));
#866=EDGE_LOOP('',(#2880));
#867=EDGE_LOOP('',(#2881));
#868=EDGE_LOOP('',(#2882,#2883,#2884,#2885));
#869=EDGE_LOOP('',(#2886,#2887,#2888,#2889));
#870=EDGE_LOOP('',(#2890));
#871=EDGE_LOOP('',(#2891));
#872=EDGE_LOOP('',(#2892));
#873=EDGE_LOOP('',(#2893));
#874=EDGE_LOOP('',(#2894,#2895,#2896,#2897));
#875=EDGE_LOOP('',(#2898,#2899,#2900,#2901));
#876=EDGE_LOOP('',(#2902,#2903,#2904,#2905));
#877=EDGE_LOOP('',(#2906,#2907,#2908,#2909));
#878=EDGE_LOOP('',(#2910,#2911,#2912,#2913));
#879=EDGE_LOOP('',(#2914,#2915,#2916,#2917));
#880=EDGE_LOOP('',(#2918));
#881=EDGE_LOOP('',(#2919));
#882=EDGE_LOOP('',(#2920));
#883=EDGE_LOOP('',(#2921));
#884=EDGE_LOOP('',(#2922));
#885=EDGE_LOOP('',(#2923));
#886=EDGE_LOOP('',(#2924));
#887=EDGE_LOOP('',(#2925));
#888=EDGE_LOOP('',(#2926));
#889=EDGE_LOOP('',(#2927));
#890=EDGE_LOOP('',(#2928));
#891=EDGE_LOOP('',(#2929));
#892=EDGE_LOOP('',(#2930,#2931,#2932,#2933));
#893=EDGE_LOOP('',(#2934,#2935,#2936,#2937));
#894=EDGE_LOOP('',(#2938,#2939,#2940,#2941));
#895=EDGE_LOOP('',(#2942,#2943,#2944,#2945));
#896=EDGE_LOOP('',(#2946,#2947,#2948,#2949));
#897=EDGE_LOOP('',(#2950,#2951,#2952,#2953));
#898=EDGE_LOOP('',(#2954));
#899=EDGE_LOOP('',(#2955));
#900=EDGE_LOOP('',(#2956,#2957,#2958,#2959));
#901=EDGE_LOOP('',(#2960));
#902=EDGE_LOOP('',(#2961));
#903=EDGE_LOOP('',(#2962));
#904=EDGE_LOOP('',(#2963));
#905=EDGE_LOOP('',(#2964));
#906=EDGE_LOOP('',(#2965));
#907=EDGE_LOOP('',(#2966));
#908=EDGE_LOOP('',(#2967));
#909=EDGE_LOOP('',(#2968));
#910=EDGE_LOOP('',(#2969));
#911=EDGE_LOOP('',(#2970));
#912=EDGE_LOOP('',(#2971));
#913=EDGE_LOOP('',(#2972));
#914=EDGE_LOOP('',(#2973,#2974,#2975,#2976));
#915=EDGE_LOOP('',(#2977,#2978,#2979,#2980));
#916=EDGE_LOOP('',(#2981,#2982,#2983,#2984));
#917=EDGE_LOOP('',(#2985));
#918=EDGE_LOOP('',(#2986));
#919=EDGE_LOOP('',(#2987,#2988,#2989,#2990));
#920=EDGE_LOOP('',(#2991,#2992,#2993,#2994));
#921=EDGE_LOOP('',(#2995,#2996,#2997,#2998));
#922=EDGE_LOOP('',(#2999));
#923=EDGE_LOOP('',(#3000,#3001,#3002,#3003));
#924=EDGE_LOOP('',(#3004,#3005,#3006,#3007));
#925=EDGE_LOOP('',(#3008,#3009,#3010,#3011));
#926=EDGE_LOOP('',(#3012,#3013,#3014,#3015));
#927=EDGE_LOOP('',(#3016,#3017,#3018,#3019));
#928=EDGE_LOOP('',(#3020,#3021,#3022,#3023));
#929=EDGE_LOOP('',(#3024,#3025,#3026,#3027,#3028,#3029));
#930=EDGE_LOOP('',(#3030,#3031,#3032,#3033,#3034,#3035));
#931=EDGE_LOOP('',(#3036,#3037,#3038,#3039,#3040,#3041));
#932=EDGE_LOOP('',(#3042));
#933=EDGE_LOOP('',(#3043,#3044,#3045,#3046,#3047,#3048));
#934=EDGE_LOOP('',(#3049));
#935=EDGE_LOOP('',(#3050,#3051,#3052,#3053));
#936=EDGE_LOOP('',(#3054,#3055,#3056,#3057));
#937=EDGE_LOOP('',(#3058,#3059,#3060,#3061));
#938=EDGE_LOOP('',(#3062,#3063,#3064,#3065));
#939=EDGE_LOOP('',(#3066,#3067,#3068,#3069));
#940=EDGE_LOOP('',(#3070,#3071,#3072,#3073));
#941=EDGE_LOOP('',(#3074,#3075,#3076,#3077));
#942=EDGE_LOOP('',(#3078));
#943=EDGE_LOOP('',(#3079));
#944=EDGE_LOOP('',(#3080,#3081,#3082,#3083));
#945=EDGE_LOOP('',(#3084,#3085,#3086,#3087));
#946=EDGE_LOOP('',(#3088,#3089,#3090,#3091));
#947=EDGE_LOOP('',(#3092));
#948=EDGE_LOOP('',(#3093));
#949=EDGE_LOOP('',(#3094,#3095,#3096,#3097));
#950=EDGE_LOOP('',(#3098,#3099,#3100,#3101,#3102,#3103));
#951=EDGE_LOOP('',(#3104));
#952=EDGE_LOOP('',(#3105,#3106,#3107,#3108));
#953=EDGE_LOOP('',(#3109,#3110,#3111,#3112));
#954=EDGE_LOOP('',(#3113,#3114,#3115,#3116));
#955=EDGE_LOOP('',(#3117,#3118,#3119,#3120));
#956=EDGE_LOOP('',(#3121,#3122,#3123,#3124));
#957=EDGE_LOOP('',(#3125,#3126,#3127,#3128));
#958=EDGE_LOOP('',(#3129,#3130,#3131,#3132,#3133,#3134));
#959=EDGE_LOOP('',(#3135,#3136,#3137,#3138));
#960=EDGE_LOOP('',(#3139));
#961=LINE('',#4497,#1124);
#962=LINE('',#4503,#1125);
#963=LINE('',#4509,#1126);
#964=LINE('',#4515,#1127);
#965=LINE('',#4525,#1128);
#966=LINE('',#4572,#1129);
#967=LINE('',#4593,#1130);
#968=LINE('',#4605,#1131);
#969=LINE('',#4654,#1132);
#970=LINE('',#4663,#1133);
#971=LINE('',#4667,#1134);
#972=LINE('',#4676,#1135);
#973=LINE('',#4679,#1136);
#974=LINE('',#4690,#1137);
#975=LINE('',#4735,#1138);
#976=LINE('',#4813,#1139);
#977=LINE('',#4891,#1140);
#978=LINE('',#4969,#1141);
#979=LINE('',#5047,#1142);
#980=LINE('',#5125,#1143);
#981=LINE('',#5203,#1144);
#982=LINE('',#5281,#1145);
#983=LINE('',#5359,#1146);
#984=LINE('',#5437,#1147);
#985=LINE('',#5515,#1148);
#986=LINE('',#5593,#1149);
#987=LINE('',#5671,#1150);
#988=LINE('',#5749,#1151);
#989=LINE('',#5827,#1152);
#990=LINE('',#5905,#1153);
#991=LINE('',#5983,#1154);
#992=LINE('',#6061,#1155);
#993=LINE('',#6139,#1156);
#994=LINE('',#6217,#1157);
#995=LINE('',#6295,#1158);
#996=LINE('',#6373,#1159);
#997=LINE('',#6451,#1160);
#998=LINE('',#6529,#1161);
#999=LINE('',#6607,#1162);
#1000=LINE('',#6685,#1163);
#1001=LINE('',#6763,#1164);
#1002=LINE('',#6841,#1165);
#1003=LINE('',#6919,#1166);
#1004=LINE('',#6997,#1167);
#1005=LINE('',#7075,#1168);
#1006=LINE('',#7153,#1169);
#1007=LINE('',#7231,#1170);
#1008=LINE('',#7309,#1171);
#1009=LINE('',#7387,#1172);
#1010=LINE('',#7465,#1173);
#1011=LINE('',#7546,#1174);
#1012=LINE('',#7627,#1175);
#1013=LINE('',#7708,#1176);
#1014=LINE('',#7789,#1177);
#1015=LINE('',#7870,#1178);
#1016=LINE('',#7951,#1179);
#1017=LINE('',#8032,#1180);
#1018=LINE('',#8113,#1181);
#1019=LINE('',#8194,#1182);
#1020=LINE('',#8275,#1183);
#1021=LINE('',#8356,#1184);
#1022=LINE('',#8437,#1185);
#1023=LINE('',#8479,#1186);
#1024=LINE('',#8484,#1187);
#1025=LINE('',#8485,#1188);
#1026=LINE('',#8486,#1189);
#1027=LINE('',#8487,#1190);
#1028=LINE('',#8488,#1191);
#1029=LINE('',#8489,#1192);
#1030=LINE('',#8491,#1193);
#1031=LINE('',#8500,#1194);
#1032=LINE('',#8504,#1195);
#1033=LINE('',#8505,#1196);
#1034=LINE('',#8506,#1197);
#1035=LINE('',#8507,#1198);
#1036=LINE('',#8508,#1199);
#1037=LINE('',#8509,#1200);
#1038=LINE('',#8511,#1201);
#1039=LINE('',#8522,#1202);
#1040=LINE('',#8525,#1203);
#1041=LINE('',#8534,#1204);
#1042=LINE('',#8540,#1205);
#1043=LINE('',#8549,#1206);
#1044=LINE('',#8555,#1207);
#1045=LINE('',#8564,#1208);
#1046=LINE('',#8570,#1209);
#1047=LINE('',#8576,#1210);
#1048=LINE('',#8582,#1211);
#1049=LINE('',#8588,#1212);
#1050=LINE('',#8594,#1213);
#1051=LINE('',#8603,#1214);
#1052=LINE('',#8609,#1215);
#1053=LINE('',#8615,#1216);
#1054=LINE('',#8621,#1217);
#1055=LINE('',#8627,#1218);
#1056=LINE('',#8633,#1219);
#1057=LINE('',#8640,#1220);
#1058=LINE('',#8651,#1221);
#1059=LINE('',#8655,#1222);
#1060=LINE('',#8659,#1223);
#1061=LINE('',#8666,#1224);
#1062=LINE('',#8670,#1225);
#1063=LINE('',#8674,#1226);
#1064=LINE('',#8679,#1227);
#1065=LINE('',#8681,#1228);
#1066=LINE('',#8683,#1229);
#1067=LINE('',#8684,#1230);
#1068=LINE('',#8687,#1231);
#1069=LINE('',#8689,#1232);
#1070=LINE('',#8690,#1233);
#1071=LINE('',#8693,#1234);
#1072=LINE('',#8695,#1235);
#1073=LINE('',#8696,#1236);
#1074=LINE('',#8699,#1237);
#1075=LINE('',#8701,#1238);
#1076=LINE('',#8702,#1239);
#1077=LINE('',#8705,#1240);
#1078=LINE('',#8707,#1241);
#1079=LINE('',#8708,#1242);
#1080=LINE('',#8710,#1243);
#1081=LINE('',#8711,#1244);
#1082=LINE('',#8718,#1245);
#1083=LINE('',#8720,#1246);
#1084=LINE('',#8722,#1247);
#1085=LINE('',#8724,#1248);
#1086=LINE('',#8726,#1249);
#1087=LINE('',#8727,#1250);
#1088=LINE('',#8733,#1251);
#1089=LINE('',#8735,#1252);
#1090=LINE('',#8737,#1253);
#1091=LINE('',#8739,#1254);
#1092=LINE('',#8741,#1255);
#1093=LINE('',#8742,#1256);
#1094=LINE('',#8746,#1257);
#1095=LINE('',#8747,#1258);
#1096=LINE('',#8749,#1259);
#1097=LINE('',#8751,#1260);
#1098=LINE('',#8753,#1261);
#1099=LINE('',#8755,#1262);
#1100=LINE('',#8759,#1263);
#1101=LINE('',#8767,#1264);
#1102=LINE('',#8771,#1265);
#1103=LINE('',#8775,#1266);
#1104=LINE('',#8780,#1267);
#1105=LINE('',#8785,#1268);
#1106=LINE('',#8787,#1269);
#1107=LINE('',#8789,#1270);
#1108=LINE('',#8791,#1271);
#1109=LINE('',#8793,#1272);
#1110=LINE('',#8794,#1273);
#1111=LINE('',#8799,#1274);
#1112=LINE('',#8801,#1275);
#1113=LINE('',#8802,#1276);
#1114=LINE('',#8805,#1277);
#1115=LINE('',#8806,#1278);
#1116=LINE('',#8809,#1279);
#1117=LINE('',#8810,#1280);
#1118=LINE('',#8813,#1281);
#1119=LINE('',#8814,#1282);
#1120=LINE('',#8817,#1283);
#1121=LINE('',#8818,#1284);
#1122=LINE('',#8820,#1285);
#1123=LINE('',#8824,#1286);
#1124=VECTOR('',#3781,0.25);
#1125=VECTOR('',#3788,0.25);
#1126=VECTOR('',#3795,0.25);
#1127=VECTOR('',#3802,0.25);
#1128=VECTOR('',#3813,1.);
#1129=VECTOR('',#3818,1.6);
#1130=VECTOR('',#3831,1.01);
#1131=VECTOR('',#3846,0.79);
#1132=VECTOR('',#3861,0.93);
#1133=VECTOR('',#3872,0.93);
#1134=VECTOR('',#3879,0.79);
#1135=VECTOR('',#3890,3.);
#1136=VECTOR('',#3893,2.);
#1137=VECTOR('',#3906,2.);
#1138=VECTOR('',#3917,0.0999999999999997);
#1139=VECTOR('',#3920,0.0999999999999997);
#1140=VECTOR('',#3923,0.0999999999999997);
#1141=VECTOR('',#3926,0.0999999999999997);
#1142=VECTOR('',#3929,0.1);
#1143=VECTOR('',#3932,0.1);
#1144=VECTOR('',#3935,0.1);
#1145=VECTOR('',#3938,0.1);
#1146=VECTOR('',#3941,0.1);
#1147=VECTOR('',#3944,0.1);
#1148=VECTOR('',#3947,0.0999999999999997);
#1149=VECTOR('',#3950,0.0999999999999997);
#1150=VECTOR('',#3953,0.0999999999999996);
#1151=VECTOR('',#3956,0.0999999999999996);
#1152=VECTOR('',#3959,0.0999999999999996);
#1153=VECTOR('',#3962,0.0999999999999996);
#1154=VECTOR('',#3965,0.1);
#1155=VECTOR('',#3968,0.1);
#1156=VECTOR('',#3971,0.1);
#1157=VECTOR('',#3974,0.1);
#1158=VECTOR('',#3977,0.1);
#1159=VECTOR('',#3980,0.1);
#1160=VECTOR('',#3983,0.0999999999999996);
#1161=VECTOR('',#3986,0.0999999999999996);
#1162=VECTOR('',#3989,0.0999999999999996);
#1163=VECTOR('',#3992,0.0999999999999996);
#1164=VECTOR('',#3995,0.0999999999999996);
#1165=VECTOR('',#3998,0.0999999999999996);
#1166=VECTOR('',#4001,0.1);
#1167=VECTOR('',#4004,0.1);
#1168=VECTOR('',#4007,0.1);
#1169=VECTOR('',#4010,0.1);
#1170=VECTOR('',#4013,0.1);
#1171=VECTOR('',#4016,0.1);
#1172=VECTOR('',#4019,0.0999999999999996);
#1173=VECTOR('',#4022,0.0999999999999996);
#1174=VECTOR('',#4025,0.0999999999999996);
#1175=VECTOR('',#4028,0.0999999999999996);
#1176=VECTOR('',#4031,0.0999999999999996);
#1177=VECTOR('',#4034,0.0999999999999996);
#1178=VECTOR('',#4037,0.1);
#1179=VECTOR('',#4040,0.1);
#1180=VECTOR('',#4043,0.1);
#1181=VECTOR('',#4046,0.1);
#1182=VECTOR('',#4049,0.1);
#1183=VECTOR('',#4052,0.1);
#1184=VECTOR('',#4055,0.0999999999999996);
#1185=VECTOR('',#4058,0.0999999999999996);
#1186=VECTOR('',#4063,0.685);
#1187=VECTOR('',#4070,1.);
#1188=VECTOR('',#4071,1.);
#1189=VECTOR('',#4072,1.);
#1190=VECTOR('',#4073,1.);
#1191=VECTOR('',#4074,1.);
#1192=VECTOR('',#4075,1.);
#1193=VECTOR('',#4076,1.);
#1194=VECTOR('',#4089,0.8);
#1195=VECTOR('',#4094,1.1);
#1196=VECTOR('',#4095,1.1);
#1197=VECTOR('',#4096,1.1);
#1198=VECTOR('',#4097,1.1);
#1199=VECTOR('',#4098,1.1);
#1200=VECTOR('',#4099,1.1);
#1201=VECTOR('',#4100,1.1);
#1202=VECTOR('',#4115,1.4);
#1203=VECTOR('',#4118,1.);
#1204=VECTOR('',#4131,1.01);
#1205=VECTOR('',#4138,1.4);
#1206=VECTOR('',#4151,0.685);
#1207=VECTOR('',#4158,1.1);
#1208=VECTOR('',#4171,0.33);
#1209=VECTOR('',#4178,0.33);
#1210=VECTOR('',#4185,0.33);
#1211=VECTOR('',#4192,0.33);
#1212=VECTOR('',#4199,1.6);
#1213=VECTOR('',#4206,3.);
#1214=VECTOR('',#4219,0.33);
#1215=VECTOR('',#4226,0.33);
#1216=VECTOR('',#4233,0.33);
#1217=VECTOR('',#4240,0.33);
#1218=VECTOR('',#4247,0.685);
#1219=VECTOR('',#4254,1.3);
#1220=VECTOR('',#4263,3.);
#1221=VECTOR('',#4280,0.475);
#1222=VECTOR('',#4285,0.5);
#1223=VECTOR('',#4290,0.485);
#1224=VECTOR('',#4299,0.31);
#1225=VECTOR('',#4304,0.3);
#1226=VECTOR('',#4309,0.27);
#1227=VECTOR('',#4314,1.);
#1228=VECTOR('',#4315,1.);
#1229=VECTOR('',#4316,1.);
#1230=VECTOR('',#4317,1.);
#1231=VECTOR('',#4320,1.);
#1232=VECTOR('',#4321,1.);
#1233=VECTOR('',#4322,1.);
#1234=VECTOR('',#4325,1.);
#1235=VECTOR('',#4326,1.);
#1236=VECTOR('',#4327,1.);
#1237=VECTOR('',#4330,1.);
#1238=VECTOR('',#4331,1.);
#1239=VECTOR('',#4332,1.);
#1240=VECTOR('',#4335,1.);
#1241=VECTOR('',#4336,1.);
#1242=VECTOR('',#4337,1.);
#1243=VECTOR('',#4340,1.);
#1244=VECTOR('',#4341,1.);
#1245=VECTOR('',#4350,1.);
#1246=VECTOR('',#4351,1.);
#1247=VECTOR('',#4352,1.);
#1248=VECTOR('',#4353,1.);
#1249=VECTOR('',#4354,1.);
#1250=VECTOR('',#4355,1.);
#1251=VECTOR('',#4360,1.);
#1252=VECTOR('',#4361,1.);
#1253=VECTOR('',#4362,1.);
#1254=VECTOR('',#4363,1.);
#1255=VECTOR('',#4364,1.);
#1256=VECTOR('',#4365,1.);
#1257=VECTOR('',#4370,1.);
#1258=VECTOR('',#4371,1.);
#1259=VECTOR('',#4374,1.);
#1260=VECTOR('',#4377,1.);
#1261=VECTOR('',#4380,1.);
#1262=VECTOR('',#4383,1.);
#1263=VECTOR('',#4388,1.065);
#1264=VECTOR('',#4399,1.025);
#1265=VECTOR('',#4404,1.065);
#1266=VECTOR('',#4409,1.025);
#1267=VECTOR('',#4416,0.79);
#1268=VECTOR('',#4421,1.);
#1269=VECTOR('',#4422,1.);
#1270=VECTOR('',#4423,1.);
#1271=VECTOR('',#4424,1.);
#1272=VECTOR('',#4425,1.);
#1273=VECTOR('',#4426,1.);
#1274=VECTOR('',#4431,1.);
#1275=VECTOR('',#4432,1.);
#1276=VECTOR('',#4433,1.);
#1277=VECTOR('',#4436,1.);
#1278=VECTOR('',#4437,1.);
#1279=VECTOR('',#4440,1.);
#1280=VECTOR('',#4441,1.);
#1281=VECTOR('',#4444,1.);
#1282=VECTOR('',#4445,1.);
#1283=VECTOR('',#4448,1.);
#1284=VECTOR('',#4449,1.);
#1285=VECTOR('',#4452,1.);
#1286=VECTOR('',#4457,0.685);
#1287=CIRCLE('',#3497,0.25);
#1288=CIRCLE('',#3498,0.25);
#1289=CIRCLE('',#3500,0.25);
#1290=CIRCLE('',#3501,0.25);
#1291=CIRCLE('',#3503,0.25);
#1292=CIRCLE('',#3504,0.25);
#1293=CIRCLE('',#3506,0.25);
#1294=CIRCLE('',#3507,0.25);
#1295=CIRCLE('',#3510,1.6);
#1296=CIRCLE('',#3512,1.01);
#1297=CIRCLE('',#3514,1.6);
#1298=CIRCLE('',#3516,0.79);
#1299=CIRCLE('',#3517,0.79);
#1300=CIRCLE('',#3519,1.01);
#1301=CIRCLE('',#3520,1.01);
#1302=CIRCLE('',#3523,0.8);
#1303=CIRCLE('',#3526,0.79);
#1304=CIRCLE('',#3530,0.8);
#1305=CIRCLE('',#3533,0.93);
#1306=CIRCLE('',#3534,0.93);
#1307=CIRCLE('',#3536,0.79);
#1308=CIRCLE('',#3538,0.93);
#1309=CIRCLE('',#3539,0.93);
#1310=CIRCLE('',#3543,3.);
#1311=CIRCLE('',#3544,2.);
#1312=CIRCLE('',#3546,3.);
#1313=CIRCLE('',#3553,2.);
#1314=CIRCLE('',#3554,2.);
#1315=CIRCLE('',#3607,0.685);
#1316=CIRCLE('',#3608,0.685);
#1317=CIRCLE('',#3610,1.);
#1318=CIRCLE('',#3611,1.);
#1319=CIRCLE('',#3614,0.8);
#1320=CIRCLE('',#3616,0.8);
#1321=CIRCLE('',#3618,1.1);
#1322=CIRCLE('',#3619,1.1);
#1323=CIRCLE('',#3622,1.4);
#1324=CIRCLE('',#3623,1.);
#1325=CIRCLE('',#3625,1.4);
#1326=CIRCLE('',#3627,1.);
#1327=CIRCLE('',#3632,1.01);
#1328=CIRCLE('',#3633,1.01);
#1329=CIRCLE('',#3635,1.4);
#1330=CIRCLE('',#3636,1.4);
#1331=CIRCLE('',#3641,0.685);
#1332=CIRCLE('',#3642,0.685);
#1333=CIRCLE('',#3644,1.1);
#1334=CIRCLE('',#3645,1.1);
#1335=CIRCLE('',#3650,0.33);
#1336=CIRCLE('',#3651,0.33);
#1337=CIRCLE('',#3653,0.33);
#1338=CIRCLE('',#3654,0.33);
#1339=CIRCLE('',#3656,0.33);
#1340=CIRCLE('',#3657,0.33);
#1341=CIRCLE('',#3659,0.33);
#1342=CIRCLE('',#3660,0.33);
#1343=CIRCLE('',#3662,1.6);
#1344=CIRCLE('',#3663,1.6);
#1345=CIRCLE('',#3665,3.);
#1346=CIRCLE('',#3666,3.);
#1347=CIRCLE('',#3671,0.33);
#1348=CIRCLE('',#3672,0.33);
#1349=CIRCLE('',#3674,0.33);
#1350=CIRCLE('',#3675,0.33);
#1351=CIRCLE('',#3677,0.33);
#1352=CIRCLE('',#3678,0.33);
#1353=CIRCLE('',#3680,0.33);
#1354=CIRCLE('',#3681,0.33);
#1355=CIRCLE('',#3683,0.685);
#1356=CIRCLE('',#3684,0.685);
#1357=CIRCLE('',#3686,1.3);
#1358=CIRCLE('',#3687,1.3);
#1359=CIRCLE('',#3690,3.);
#1360=CIRCLE('',#3691,3.);
#1361=CIRCLE('',#3696,0.45);
#1362=CIRCLE('',#3698,0.5);
#1363=CIRCLE('',#3700,0.5);
#1364=CIRCLE('',#3702,0.47);
#1365=CIRCLE('',#3704,0.32);
#1366=CIRCLE('',#3706,0.2942);
#1367=CIRCLE('',#3708,0.2942);
#1368=CIRCLE('',#3710,0.24);
#1369=CIRCLE('',#3722,1.065);
#1370=CIRCLE('',#3724,1.065);
#1371=CIRCLE('',#3732,1.065);
#1372=CIRCLE('',#3734,0.985);
#1373=CIRCLE('',#3735,0.79);
#1374=CIRCLE('',#3738,1.065);
#1375=CIRCLE('',#3740,0.985);
#1376=CIRCLE('',#3742,0.79);
#1377=CIRCLE('',#3746,0.685);
#1378=CIRCLE('',#3755,0.685);
#1379=VERTEX_POINT('',#4494);
#1380=VERTEX_POINT('',#4496);
#1381=VERTEX_POINT('',#4500);
#1382=VERTEX_POINT('',#4502);
#1383=VERTEX_POINT('',#4506);
#1384=VERTEX_POINT('',#4508);
#1385=VERTEX_POINT('',#4512);
#1386=VERTEX_POINT('',#4514);
#1387=VERTEX_POINT('',#4518);
#1388=VERTEX_POINT('',#4519);
#1389=VERTEX_POINT('',#4521);
#1390=VERTEX_POINT('',#4523);
#1391=VERTEX_POINT('',#4526);
#1392=VERTEX_POINT('',#4529);
#1393=VERTEX_POINT('',#4571);
#1394=VERTEX_POINT('',#4575);
#1395=VERTEX_POINT('',#4579);
#1396=VERTEX_POINT('',#4580);
#1397=VERTEX_POINT('',#4591);
#1398=VERTEX_POINT('',#4596);
#1399=VERTEX_POINT('',#4598);
#1400=VERTEX_POINT('',#4602);
#1401=VERTEX_POINT('',#4604);
#1402=VERTEX_POINT('',#4606);
#1403=VERTEX_POINT('',#4627);
#1404=VERTEX_POINT('',#4651);
#1405=VERTEX_POINT('',#4653);
#1406=VERTEX_POINT('',#4657);
#1407=VERTEX_POINT('',#4660);
#1408=VERTEX_POINT('',#4662);
#1409=VERTEX_POINT('',#4669);
#1410=VERTEX_POINT('',#4671);
#1411=VERTEX_POINT('',#4674);
#1412=VERTEX_POINT('',#4678);
#1413=VERTEX_POINT('',#4680);
#1414=VERTEX_POINT('',#4682);
#1415=VERTEX_POINT('',#4687);
#1416=VERTEX_POINT('',#4689);
#1417=VERTEX_POINT('',#4696);
#1418=VERTEX_POINT('',#4697);
#1419=VERTEX_POINT('',#4734);
#1420=VERTEX_POINT('',#4736);
#1421=VERTEX_POINT('',#4774);
#1422=VERTEX_POINT('',#4775);
#1423=VERTEX_POINT('',#4812);
#1424=VERTEX_POINT('',#4814);
#1425=VERTEX_POINT('',#4852);
#1426=VERTEX_POINT('',#4853);
#1427=VERTEX_POINT('',#4890);
#1428=VERTEX_POINT('',#4892);
#1429=VERTEX_POINT('',#4930);
#1430=VERTEX_POINT('',#4931);
#1431=VERTEX_POINT('',#4968);
#1432=VERTEX_POINT('',#4970);
#1433=VERTEX_POINT('',#5008);
#1434=VERTEX_POINT('',#5009);
#1435=VERTEX_POINT('',#5046);
#1436=VERTEX_POINT('',#5048);
#1437=VERTEX_POINT('',#5086);
#1438=VERTEX_POINT('',#5087);
#1439=VERTEX_POINT('',#5124);
#1440=VERTEX_POINT('',#5126);
#1441=VERTEX_POINT('',#5164);
#1442=VERTEX_POINT('',#5165);
#1443=VERTEX_POINT('',#5202);
#1444=VERTEX_POINT('',#5204);
#1445=VERTEX_POINT('',#5242);
#1446=VERTEX_POINT('',#5243);
#1447=VERTEX_POINT('',#5280);
#1448=VERTEX_POINT('',#5282);
#1449=VERTEX_POINT('',#5320);
#1450=VERTEX_POINT('',#5321);
#1451=VERTEX_POINT('',#5358);
#1452=VERTEX_POINT('',#5360);
#1453=VERTEX_POINT('',#5398);
#1454=VERTEX_POINT('',#5399);
#1455=VERTEX_POINT('',#5436);
#1456=VERTEX_POINT('',#5438);
#1457=VERTEX_POINT('',#5476);
#1458=VERTEX_POINT('',#5477);
#1459=VERTEX_POINT('',#5514);
#1460=VERTEX_POINT('',#5516);
#1461=VERTEX_POINT('',#5554);
#1462=VERTEX_POINT('',#5555);
#1463=VERTEX_POINT('',#5592);
#1464=VERTEX_POINT('',#5594);
#1465=VERTEX_POINT('',#5632);
#1466=VERTEX_POINT('',#5633);
#1467=VERTEX_POINT('',#5670);
#1468=VERTEX_POINT('',#5672);
#1469=VERTEX_POINT('',#5710);
#1470=VERTEX_POINT('',#5711);
#1471=VERTEX_POINT('',#5748);
#1472=VERTEX_POINT('',#5750);
#1473=VERTEX_POINT('',#5788);
#1474=VERTEX_POINT('',#5789);
#1475=VERTEX_POINT('',#5826);
#1476=VERTEX_POINT('',#5828);
#1477=VERTEX_POINT('',#5866);
#1478=VERTEX_POINT('',#5867);
#1479=VERTEX_POINT('',#5904);
#1480=VERTEX_POINT('',#5906);
#1481=VERTEX_POINT('',#5944);
#1482=VERTEX_POINT('',#5945);
#1483=VERTEX_POINT('',#5982);
#1484=VERTEX_POINT('',#5984);
#1485=VERTEX_POINT('',#6022);
#1486=VERTEX_POINT('',#6023);
#1487=VERTEX_POINT('',#6060);
#1488=VERTEX_POINT('',#6062);
#1489=VERTEX_POINT('',#6100);
#1490=VERTEX_POINT('',#6101);
#1491=VERTEX_POINT('',#6138);
#1492=VERTEX_POINT('',#6140);
#1493=VERTEX_POINT('',#6178);
#1494=VERTEX_POINT('',#6179);
#1495=VERTEX_POINT('',#6216);
#1496=VERTEX_POINT('',#6218);
#1497=VERTEX_POINT('',#6256);
#1498=VERTEX_POINT('',#6257);
#1499=VERTEX_POINT('',#6294);
#1500=VERTEX_POINT('',#6296);
#1501=VERTEX_POINT('',#6334);
#1502=VERTEX_POINT('',#6335);
#1503=VERTEX_POINT('',#6372);
#1504=VERTEX_POINT('',#6374);
#1505=VERTEX_POINT('',#6412);
#1506=VERTEX_POINT('',#6413);
#1507=VERTEX_POINT('',#6450);
#1508=VERTEX_POINT('',#6452);
#1509=VERTEX_POINT('',#6490);
#1510=VERTEX_POINT('',#6491);
#1511=VERTEX_POINT('',#6528);
#1512=VERTEX_POINT('',#6530);
#1513=VERTEX_POINT('',#6568);
#1514=VERTEX_POINT('',#6569);
#1515=VERTEX_POINT('',#6606);
#1516=VERTEX_POINT('',#6608);
#1517=VERTEX_POINT('',#6646);
#1518=VERTEX_POINT('',#6647);
#1519=VERTEX_POINT('',#6684);
#1520=VERTEX_POINT('',#6686);
#1521=VERTEX_POINT('',#6724);
#1522=VERTEX_POINT('',#6725);
#1523=VERTEX_POINT('',#6762);
#1524=VERTEX_POINT('',#6764);
#1525=VERTEX_POINT('',#6802);
#1526=VERTEX_POINT('',#6803);
#1527=VERTEX_POINT('',#6840);
#1528=VERTEX_POINT('',#6842);
#1529=VERTEX_POINT('',#6880);
#1530=VERTEX_POINT('',#6881);
#1531=VERTEX_POINT('',#6918);
#1532=VERTEX_POINT('',#6920);
#1533=VERTEX_POINT('',#6958);
#1534=VERTEX_POINT('',#6959);
#1535=VERTEX_POINT('',#6996);
#1536=VERTEX_POINT('',#6998);
#1537=VERTEX_POINT('',#7036);
#1538=VERTEX_POINT('',#7037);
#1539=VERTEX_POINT('',#7074);
#1540=VERTEX_POINT('',#7076);
#1541=VERTEX_POINT('',#7114);
#1542=VERTEX_POINT('',#7115);
#1543=VERTEX_POINT('',#7152);
#1544=VERTEX_POINT('',#7154);
#1545=VERTEX_POINT('',#7192);
#1546=VERTEX_POINT('',#7193);
#1547=VERTEX_POINT('',#7230);
#1548=VERTEX_POINT('',#7232);
#1549=VERTEX_POINT('',#7270);
#1550=VERTEX_POINT('',#7271);
#1551=VERTEX_POINT('',#7308);
#1552=VERTEX_POINT('',#7310);
#1553=VERTEX_POINT('',#7348);
#1554=VERTEX_POINT('',#7349);
#1555=VERTEX_POINT('',#7386);
#1556=VERTEX_POINT('',#7388);
#1557=VERTEX_POINT('',#7426);
#1558=VERTEX_POINT('',#7427);
#1559=VERTEX_POINT('',#7464);
#1560=VERTEX_POINT('',#7466);
#1561=VERTEX_POINT('',#7504);
#1562=VERTEX_POINT('',#7505);
#1563=VERTEX_POINT('',#7516);
#1564=VERTEX_POINT('',#7545);
#1565=VERTEX_POINT('',#7547);
#1566=VERTEX_POINT('',#7566);
#1567=VERTEX_POINT('',#7588);
#1568=VERTEX_POINT('',#7589);
#1569=VERTEX_POINT('',#7626);
#1570=VERTEX_POINT('',#7628);
#1571=VERTEX_POINT('',#7666);
#1572=VERTEX_POINT('',#7667);
#1573=VERTEX_POINT('',#7678);
#1574=VERTEX_POINT('',#7707);
#1575=VERTEX_POINT('',#7709);
#1576=VERTEX_POINT('',#7728);
#1577=VERTEX_POINT('',#7750);
#1578=VERTEX_POINT('',#7751);
#1579=VERTEX_POINT('',#7788);
#1580=VERTEX_POINT('',#7790);
#1581=VERTEX_POINT('',#7828);
#1582=VERTEX_POINT('',#7829);
#1583=VERTEX_POINT('',#7840);
#1584=VERTEX_POINT('',#7869);
#1585=VERTEX_POINT('',#7871);
#1586=VERTEX_POINT('',#7890);
#1587=VERTEX_POINT('',#7912);
#1588=VERTEX_POINT('',#7913);
#1589=VERTEX_POINT('',#7950);
#1590=VERTEX_POINT('',#7952);
#1591=VERTEX_POINT('',#7990);
#1592=VERTEX_POINT('',#7991);
#1593=VERTEX_POINT('',#8002);
#1594=VERTEX_POINT('',#8031);
#1595=VERTEX_POINT('',#8033);
#1596=VERTEX_POINT('',#8052);
#1597=VERTEX_POINT('',#8074);
#1598=VERTEX_POINT('',#8075);
#1599=VERTEX_POINT('',#8112);
#1600=VERTEX_POINT('',#8114);
#1601=VERTEX_POINT('',#8152);
#1602=VERTEX_POINT('',#8153);
#1603=VERTEX_POINT('',#8164);
#1604=VERTEX_POINT('',#8193);
#1605=VERTEX_POINT('',#8195);
#1606=VERTEX_POINT('',#8214);
#1607=VERTEX_POINT('',#8236);
#1608=VERTEX_POINT('',#8237);
#1609=VERTEX_POINT('',#8274);
#1610=VERTEX_POINT('',#8276);
#1611=VERTEX_POINT('',#8314);
#1612=VERTEX_POINT('',#8315);
#1613=VERTEX_POINT('',#8326);
#1614=VERTEX_POINT('',#8355);
#1615=VERTEX_POINT('',#8357);
#1616=VERTEX_POINT('',#8376);
#1617=VERTEX_POINT('',#8398);
#1618=VERTEX_POINT('',#8399);
#1619=VERTEX_POINT('',#8436);
#1620=VERTEX_POINT('',#8438);
#1621=VERTEX_POINT('',#8476);
#1622=VERTEX_POINT('',#8478);
#1623=VERTEX_POINT('',#8482);
#1624=VERTEX_POINT('',#8490);
#1625=VERTEX_POINT('',#8495);
#1626=VERTEX_POINT('',#8498);
#1627=VERTEX_POINT('',#8502);
#1628=VERTEX_POINT('',#8510);
#1629=VERTEX_POINT('',#8515);
#1630=VERTEX_POINT('',#8517);
#1631=VERTEX_POINT('',#8520);
#1632=VERTEX_POINT('',#8524);
#1633=VERTEX_POINT('',#8531);
#1634=VERTEX_POINT('',#8533);
#1635=VERTEX_POINT('',#8537);
#1636=VERTEX_POINT('',#8539);
#1637=VERTEX_POINT('',#8546);
#1638=VERTEX_POINT('',#8548);
#1639=VERTEX_POINT('',#8552);
#1640=VERTEX_POINT('',#8554);
#1641=VERTEX_POINT('',#8561);
#1642=VERTEX_POINT('',#8563);
#1643=VERTEX_POINT('',#8567);
#1644=VERTEX_POINT('',#8569);
#1645=VERTEX_POINT('',#8573);
#1646=VERTEX_POINT('',#8575);
#1647=VERTEX_POINT('',#8579);
#1648=VERTEX_POINT('',#8581);
#1649=VERTEX_POINT('',#8585);
#1650=VERTEX_POINT('',#8587);
#1651=VERTEX_POINT('',#8591);
#1652=VERTEX_POINT('',#8593);
#1653=VERTEX_POINT('',#8600);
#1654=VERTEX_POINT('',#8602);
#1655=VERTEX_POINT('',#8606);
#1656=VERTEX_POINT('',#8608);
#1657=VERTEX_POINT('',#8612);
#1658=VERTEX_POINT('',#8614);
#1659=VERTEX_POINT('',#8618);
#1660=VERTEX_POINT('',#8620);
#1661=VERTEX_POINT('',#8624);
#1662=VERTEX_POINT('',#8626);
#1663=VERTEX_POINT('',#8630);
#1664=VERTEX_POINT('',#8632);
#1665=VERTEX_POINT('',#8637);
#1666=VERTEX_POINT('',#8639);
#1667=VERTEX_POINT('',#8646);
#1668=VERTEX_POINT('',#8649);
#1669=VERTEX_POINT('',#8653);
#1670=VERTEX_POINT('',#8657);
#1671=VERTEX_POINT('',#8661);
#1672=VERTEX_POINT('',#8664);
#1673=VERTEX_POINT('',#8668);
#1674=VERTEX_POINT('',#8672);
#1675=VERTEX_POINT('',#8677);
#1676=VERTEX_POINT('',#8678);
#1677=VERTEX_POINT('',#8680);
#1678=VERTEX_POINT('',#8682);
#1679=VERTEX_POINT('',#8686);
#1680=VERTEX_POINT('',#8688);
#1681=VERTEX_POINT('',#8692);
#1682=VERTEX_POINT('',#8694);
#1683=VERTEX_POINT('',#8698);
#1684=VERTEX_POINT('',#8700);
#1685=VERTEX_POINT('',#8704);
#1686=VERTEX_POINT('',#8706);
#1687=VERTEX_POINT('',#8716);
#1688=VERTEX_POINT('',#8717);
#1689=VERTEX_POINT('',#8719);
#1690=VERTEX_POINT('',#8721);
#1691=VERTEX_POINT('',#8723);
#1692=VERTEX_POINT('',#8725);
#1693=VERTEX_POINT('',#8728);
#1694=VERTEX_POINT('',#8731);
#1695=VERTEX_POINT('',#8732);
#1696=VERTEX_POINT('',#8734);
#1697=VERTEX_POINT('',#8736);
#1698=VERTEX_POINT('',#8738);
#1699=VERTEX_POINT('',#8740);
#1700=VERTEX_POINT('',#8743);
#1701=VERTEX_POINT('',#8758);
#1702=VERTEX_POINT('',#8762);
#1703=VERTEX_POINT('',#8764);
#1704=VERTEX_POINT('',#8769);
#1705=VERTEX_POINT('',#8773);
#1706=VERTEX_POINT('',#8777);
#1707=VERTEX_POINT('',#8783);
#1708=VERTEX_POINT('',#8784);
#1709=VERTEX_POINT('',#8786);
#1710=VERTEX_POINT('',#8788);
#1711=VERTEX_POINT('',#8790);
#1712=VERTEX_POINT('',#8792);
#1713=VERTEX_POINT('',#8795);
#1714=VERTEX_POINT('',#8798);
#1715=VERTEX_POINT('',#8800);
#1716=VERTEX_POINT('',#8804);
#1717=VERTEX_POINT('',#8808);
#1718=VERTEX_POINT('',#8812);
#1719=VERTEX_POINT('',#8816);
#1720=VERTEX_POINT('',#8823);
#1721=EDGE_CURVE('',#1379,#1379,#1287,.T.);
#1722=EDGE_CURVE('',#1379,#1380,#961,.T.);
#1723=EDGE_CURVE('',#1380,#1380,#1288,.T.);
#1724=EDGE_CURVE('',#1381,#1381,#1289,.T.);
#1725=EDGE_CURVE('',#1381,#1382,#962,.T.);
#1726=EDGE_CURVE('',#1382,#1382,#1290,.T.);
#1727=EDGE_CURVE('',#1383,#1383,#1291,.T.);
#1728=EDGE_CURVE('',#1383,#1384,#963,.T.);
#1729=EDGE_CURVE('',#1384,#1384,#1292,.T.);
#1730=EDGE_CURVE('',#1385,#1385,#1293,.T.);
#1731=EDGE_CURVE('',#1385,#1386,#964,.T.);
#1732=EDGE_CURVE('',#1386,#1386,#1294,.T.);
#1733=EDGE_CURVE('',#1387,#1388,#456,.T.);
#1734=EDGE_CURVE('',#1387,#1389,#1295,.T.);
#1735=EDGE_CURVE('',#1390,#1389,#457,.T.);
#1736=EDGE_CURVE('',#1388,#1390,#965,.T.);
#1737=EDGE_CURVE('',#1391,#1391,#1296,.T.);
#1738=EDGE_CURVE('',#1389,#1392,#110,.T.);
#1739=EDGE_CURVE('',#1392,#1387,#111,.T.);
#1740=EDGE_CURVE('',#1392,#1393,#966,.T.);
#1741=EDGE_CURVE('',#1393,#1393,#1297,.T.);
#1742=EDGE_CURVE('',#1390,#1394,#1298,.T.);
#1743=EDGE_CURVE('',#1394,#1388,#1299,.T.);
#1744=EDGE_CURVE('',#1395,#1396,#112,.T.);
#1745=EDGE_CURVE('',#1397,#1395,#1300,.T.);
#1746=EDGE_CURVE('',#1397,#1391,#967,.T.);
#1747=EDGE_CURVE('',#1396,#1397,#1301,.T.);
#1748=EDGE_CURVE('',#1398,#1395,#458,.T.);
#1749=EDGE_CURVE('',#1399,#1398,#1302,.T.);
#1750=EDGE_CURVE('',#1396,#1399,#459,.T.);
#1751=EDGE_CURVE('',#1400,#1400,#1303,.T.);
#1752=EDGE_CURVE('',#1400,#1401,#968,.T.);
#1753=EDGE_CURVE('',#1401,#1402,#460,.T.);
#1754=EDGE_CURVE('',#1402,#1398,#113,.T.);
#1755=EDGE_CURVE('',#1399,#1403,#114,.T.);
#1756=EDGE_CURVE('',#1403,#1401,#461,.T.);
#1757=EDGE_CURVE('',#1403,#1402,#1304,.T.);
#1758=EDGE_CURVE('',#1404,#1404,#1305,.T.);
#1759=EDGE_CURVE('',#1404,#1405,#969,.T.);
#1760=EDGE_CURVE('',#1405,#1405,#1306,.T.);
#1761=EDGE_CURVE('',#1406,#1406,#1307,.T.);
#1762=EDGE_CURVE('',#1407,#1407,#1308,.T.);
#1763=EDGE_CURVE('',#1407,#1408,#970,.T.);
#1764=EDGE_CURVE('',#1408,#1408,#1309,.T.);
#1765=EDGE_CURVE('',#1394,#1406,#971,.T.);
#1766=EDGE_CURVE('',#1409,#1409,#1310,.T.);
#1767=EDGE_CURVE('',#1410,#1410,#1311,.T.);
#1768=EDGE_CURVE('',#1411,#1411,#1312,.T.);
#1769=EDGE_CURVE('',#1411,#1409,#972,.T.);
#1770=EDGE_CURVE('',#1410,#1412,#973,.T.);
#1771=EDGE_CURVE('',#1413,#1412,#462,.T.);
#1772=EDGE_CURVE('',#1414,#1413,#463,.T.);
#1773=EDGE_CURVE('',#1412,#1414,#464,.T.);
#1774=EDGE_CURVE('',#1415,#1415,#1313,.T.);
#1775=EDGE_CURVE('',#1415,#1416,#974,.T.);
#1776=EDGE_CURVE('',#1416,#1416,#1314,.T.);
#1777=EDGE_CURVE('',#1417,#1418,#115,.T.);
#1778=EDGE_CURVE('',#1418,#1417,#116,.T.);
#1779=EDGE_CURVE('',#1418,#1419,#975,.T.);
#1780=EDGE_CURVE('',#1420,#1419,#117,.T.);
#1781=EDGE_CURVE('',#1419,#1420,#118,.T.);
#1782=EDGE_CURVE('',#1421,#1422,#119,.T.);
#1783=EDGE_CURVE('',#1422,#1421,#120,.T.);
#1784=EDGE_CURVE('',#1422,#1423,#976,.T.);
#1785=EDGE_CURVE('',#1424,#1423,#121,.T.);
#1786=EDGE_CURVE('',#1423,#1424,#122,.T.);
#1787=EDGE_CURVE('',#1425,#1426,#123,.T.);
#1788=EDGE_CURVE('',#1426,#1425,#124,.T.);
#1789=EDGE_CURVE('',#1426,#1427,#977,.T.);
#1790=EDGE_CURVE('',#1428,#1427,#125,.T.);
#1791=EDGE_CURVE('',#1427,#1428,#126,.T.);
#1792=EDGE_CURVE('',#1429,#1430,#127,.T.);
#1793=EDGE_CURVE('',#1430,#1429,#128,.T.);
#1794=EDGE_CURVE('',#1430,#1431,#978,.T.);
#1795=EDGE_CURVE('',#1432,#1431,#129,.T.);
#1796=EDGE_CURVE('',#1431,#1432,#130,.T.);
#1797=EDGE_CURVE('',#1433,#1434,#131,.T.);
#1798=EDGE_CURVE('',#1434,#1433,#132,.T.);
#1799=EDGE_CURVE('',#1434,#1435,#979,.T.);
#1800=EDGE_CURVE('',#1436,#1435,#133,.T.);
#1801=EDGE_CURVE('',#1435,#1436,#134,.T.);
#1802=EDGE_CURVE('',#1437,#1438,#135,.T.);
#1803=EDGE_CURVE('',#1438,#1437,#136,.T.);
#1804=EDGE_CURVE('',#1438,#1439,#980,.T.);
#1805=EDGE_CURVE('',#1440,#1439,#137,.T.);
#1806=EDGE_CURVE('',#1439,#1440,#138,.T.);
#1807=EDGE_CURVE('',#1441,#1442,#139,.T.);
#1808=EDGE_CURVE('',#1442,#1441,#140,.T.);
#1809=EDGE_CURVE('',#1442,#1443,#981,.T.);
#1810=EDGE_CURVE('',#1444,#1443,#141,.T.);
#1811=EDGE_CURVE('',#1443,#1444,#142,.T.);
#1812=EDGE_CURVE('',#1445,#1446,#143,.T.);
#1813=EDGE_CURVE('',#1446,#1445,#144,.T.);
#1814=EDGE_CURVE('',#1446,#1447,#982,.T.);
#1815=EDGE_CURVE('',#1448,#1447,#145,.T.);
#1816=EDGE_CURVE('',#1447,#1448,#146,.T.);
#1817=EDGE_CURVE('',#1449,#1450,#147,.T.);
#1818=EDGE_CURVE('',#1450,#1449,#148,.T.);
#1819=EDGE_CURVE('',#1450,#1451,#983,.T.);
#1820=EDGE_CURVE('',#1452,#1451,#149,.T.);
#1821=EDGE_CURVE('',#1451,#1452,#150,.T.);
#1822=EDGE_CURVE('',#1453,#1454,#151,.T.);
#1823=EDGE_CURVE('',#1454,#1453,#152,.T.);
#1824=EDGE_CURVE('',#1454,#1455,#984,.T.);
#1825=EDGE_CURVE('',#1456,#1455,#153,.T.);
#1826=EDGE_CURVE('',#1455,#1456,#154,.T.);
#1827=EDGE_CURVE('',#1457,#1458,#155,.T.);
#1828=EDGE_CURVE('',#1458,#1457,#156,.T.);
#1829=EDGE_CURVE('',#1458,#1459,#985,.T.);
#1830=EDGE_CURVE('',#1460,#1459,#157,.T.);
#1831=EDGE_CURVE('',#1459,#1460,#158,.T.);
#1832=EDGE_CURVE('',#1461,#1462,#159,.T.);
#1833=EDGE_CURVE('',#1462,#1461,#160,.T.);
#1834=EDGE_CURVE('',#1462,#1463,#986,.T.);
#1835=EDGE_CURVE('',#1464,#1463,#161,.T.);
#1836=EDGE_CURVE('',#1463,#1464,#162,.T.);
#1837=EDGE_CURVE('',#1465,#1466,#163,.T.);
#1838=EDGE_CURVE('',#1466,#1465,#164,.T.);
#1839=EDGE_CURVE('',#1466,#1467,#987,.T.);
#1840=EDGE_CURVE('',#1468,#1467,#165,.T.);
#1841=EDGE_CURVE('',#1467,#1468,#166,.T.);
#1842=EDGE_CURVE('',#1469,#1470,#167,.T.);
#1843=EDGE_CURVE('',#1470,#1469,#168,.T.);
#1844=EDGE_CURVE('',#1470,#1471,#988,.T.);
#1845=EDGE_CURVE('',#1472,#1471,#169,.T.);
#1846=EDGE_CURVE('',#1471,#1472,#170,.T.);
#1847=EDGE_CURVE('',#1473,#1474,#171,.T.);
#1848=EDGE_CURVE('',#1474,#1473,#172,.T.);
#1849=EDGE_CURVE('',#1474,#1475,#989,.T.);
#1850=EDGE_CURVE('',#1476,#1475,#173,.T.);
#1851=EDGE_CURVE('',#1475,#1476,#174,.T.);
#1852=EDGE_CURVE('',#1477,#1478,#175,.T.);
#1853=EDGE_CURVE('',#1478,#1477,#176,.T.);
#1854=EDGE_CURVE('',#1478,#1479,#990,.T.);
#1855=EDGE_CURVE('',#1480,#1479,#177,.T.);
#1856=EDGE_CURVE('',#1479,#1480,#178,.T.);
#1857=EDGE_CURVE('',#1481,#1482,#179,.T.);
#1858=EDGE_CURVE('',#1482,#1481,#180,.T.);
#1859=EDGE_CURVE('',#1482,#1483,#991,.T.);
#1860=EDGE_CURVE('',#1484,#1483,#181,.T.);
#1861=EDGE_CURVE('',#1483,#1484,#182,.T.);
#1862=EDGE_CURVE('',#1485,#1486,#183,.T.);
#1863=EDGE_CURVE('',#1486,#1485,#184,.T.);
#1864=EDGE_CURVE('',#1486,#1487,#992,.T.);
#1865=EDGE_CURVE('',#1488,#1487,#185,.T.);
#1866=EDGE_CURVE('',#1487,#1488,#186,.T.);
#1867=EDGE_CURVE('',#1489,#1490,#187,.T.);
#1868=EDGE_CURVE('',#1490,#1489,#188,.T.);
#1869=EDGE_CURVE('',#1490,#1491,#993,.T.);
#1870=EDGE_CURVE('',#1492,#1491,#189,.T.);
#1871=EDGE_CURVE('',#1491,#1492,#190,.T.);
#1872=EDGE_CURVE('',#1493,#1494,#191,.T.);
#1873=EDGE_CURVE('',#1494,#1493,#192,.T.);
#1874=EDGE_CURVE('',#1494,#1495,#994,.T.);
#1875=EDGE_CURVE('',#1496,#1495,#193,.T.);
#1876=EDGE_CURVE('',#1495,#1496,#194,.T.);
#1877=EDGE_CURVE('',#1497,#1498,#195,.T.);
#1878=EDGE_CURVE('',#1498,#1497,#196,.T.);
#1879=EDGE_CURVE('',#1498,#1499,#995,.T.);
#1880=EDGE_CURVE('',#1500,#1499,#197,.T.);
#1881=EDGE_CURVE('',#1499,#1500,#198,.T.);
#1882=EDGE_CURVE('',#1501,#1502,#199,.T.);
#1883=EDGE_CURVE('',#1502,#1501,#200,.T.);
#1884=EDGE_CURVE('',#1502,#1503,#996,.T.);
#1885=EDGE_CURVE('',#1504,#1503,#201,.T.);
#1886=EDGE_CURVE('',#1503,#1504,#202,.T.);
#1887=EDGE_CURVE('',#1505,#1506,#203,.T.);
#1888=EDGE_CURVE('',#1506,#1505,#204,.T.);
#1889=EDGE_CURVE('',#1506,#1507,#997,.T.);
#1890=EDGE_CURVE('',#1508,#1507,#205,.T.);
#1891=EDGE_CURVE('',#1507,#1508,#206,.T.);
#1892=EDGE_CURVE('',#1509,#1510,#207,.T.);
#1893=EDGE_CURVE('',#1510,#1509,#208,.T.);
#1894=EDGE_CURVE('',#1510,#1511,#998,.T.);
#1895=EDGE_CURVE('',#1512,#1511,#209,.T.);
#1896=EDGE_CURVE('',#1511,#1512,#210,.T.);
#1897=EDGE_CURVE('',#1513,#1514,#211,.T.);
#1898=EDGE_CURVE('',#1514,#1513,#212,.T.);
#1899=EDGE_CURVE('',#1514,#1515,#999,.T.);
#1900=EDGE_CURVE('',#1516,#1515,#213,.T.);
#1901=EDGE_CURVE('',#1515,#1516,#214,.T.);
#1902=EDGE_CURVE('',#1517,#1518,#215,.T.);
#1903=EDGE_CURVE('',#1518,#1517,#216,.T.);
#1904=EDGE_CURVE('',#1518,#1519,#1000,.T.);
#1905=EDGE_CURVE('',#1520,#1519,#217,.T.);
#1906=EDGE_CURVE('',#1519,#1520,#218,.T.);
#1907=EDGE_CURVE('',#1521,#1522,#219,.T.);
#1908=EDGE_CURVE('',#1522,#1521,#220,.T.);
#1909=EDGE_CURVE('',#1522,#1523,#1001,.T.);
#1910=EDGE_CURVE('',#1524,#1523,#221,.T.);
#1911=EDGE_CURVE('',#1523,#1524,#222,.T.);
#1912=EDGE_CURVE('',#1525,#1526,#223,.T.);
#1913=EDGE_CURVE('',#1526,#1525,#224,.T.);
#1914=EDGE_CURVE('',#1526,#1527,#1002,.T.);
#1915=EDGE_CURVE('',#1528,#1527,#225,.T.);
#1916=EDGE_CURVE('',#1527,#1528,#226,.T.);
#1917=EDGE_CURVE('',#1529,#1530,#227,.T.);
#1918=EDGE_CURVE('',#1530,#1529,#228,.T.);
#1919=EDGE_CURVE('',#1530,#1531,#1003,.T.);
#1920=EDGE_CURVE('',#1532,#1531,#229,.T.);
#1921=EDGE_CURVE('',#1531,#1532,#230,.T.);
#1922=EDGE_CURVE('',#1533,#1534,#231,.T.);
#1923=EDGE_CURVE('',#1534,#1533,#232,.T.);
#1924=EDGE_CURVE('',#1534,#1535,#1004,.T.);
#1925=EDGE_CURVE('',#1536,#1535,#233,.T.);
#1926=EDGE_CURVE('',#1535,#1536,#234,.T.);
#1927=EDGE_CURVE('',#1537,#1538,#235,.T.);
#1928=EDGE_CURVE('',#1538,#1537,#236,.T.);
#1929=EDGE_CURVE('',#1538,#1539,#1005,.T.);
#1930=EDGE_CURVE('',#1540,#1539,#237,.T.);
#1931=EDGE_CURVE('',#1539,#1540,#238,.T.);
#1932=EDGE_CURVE('',#1541,#1542,#239,.T.);
#1933=EDGE_CURVE('',#1542,#1541,#240,.T.);
#1934=EDGE_CURVE('',#1542,#1543,#1006,.T.);
#1935=EDGE_CURVE('',#1544,#1543,#241,.T.);
#1936=EDGE_CURVE('',#1543,#1544,#242,.T.);
#1937=EDGE_CURVE('',#1545,#1546,#243,.T.);
#1938=EDGE_CURVE('',#1546,#1545,#244,.T.);
#1939=EDGE_CURVE('',#1546,#1547,#1007,.T.);
#1940=EDGE_CURVE('',#1548,#1547,#245,.T.);
#1941=EDGE_CURVE('',#1547,#1548,#246,.T.);
#1942=EDGE_CURVE('',#1549,#1550,#247,.T.);
#1943=EDGE_CURVE('',#1550,#1549,#248,.T.);
#1944=EDGE_CURVE('',#1550,#1551,#1008,.T.);
#1945=EDGE_CURVE('',#1552,#1551,#249,.T.);
#1946=EDGE_CURVE('',#1551,#1552,#250,.T.);
#1947=EDGE_CURVE('',#1553,#1554,#251,.T.);
#1948=EDGE_CURVE('',#1554,#1553,#252,.T.);
#1949=EDGE_CURVE('',#1554,#1555,#1009,.T.);
#1950=EDGE_CURVE('',#1556,#1555,#253,.T.);
#1951=EDGE_CURVE('',#1555,#1556,#254,.T.);
#1952=EDGE_CURVE('',#1557,#1558,#255,.T.);
#1953=EDGE_CURVE('',#1558,#1557,#256,.T.);
#1954=EDGE_CURVE('',#1558,#1559,#1010,.T.);
#1955=EDGE_CURVE('',#1560,#1559,#257,.T.);
#1956=EDGE_CURVE('',#1559,#1560,#258,.T.);
#1957=EDGE_CURVE('',#1561,#1562,#259,.T.);
#1958=EDGE_CURVE('',#1563,#1561,#260,.T.);
#1959=EDGE_CURVE('',#1562,#1563,#261,.T.);
#1960=EDGE_CURVE('',#1562,#1564,#1011,.T.);
#1961=EDGE_CURVE('',#1565,#1564,#262,.T.);
#1962=EDGE_CURVE('',#1566,#1565,#263,.T.);
#1963=EDGE_CURVE('',#1564,#1566,#264,.T.);
#1964=EDGE_CURVE('',#1567,#1568,#265,.T.);
#1965=EDGE_CURVE('',#1568,#1567,#266,.T.);
#1966=EDGE_CURVE('',#1568,#1569,#1012,.T.);
#1967=EDGE_CURVE('',#1570,#1569,#267,.T.);
#1968=EDGE_CURVE('',#1569,#1570,#268,.T.);
#1969=EDGE_CURVE('',#1571,#1572,#269,.T.);
#1970=EDGE_CURVE('',#1573,#1571,#270,.T.);
#1971=EDGE_CURVE('',#1572,#1573,#271,.T.);
#1972=EDGE_CURVE('',#1572,#1574,#1013,.T.);
#1973=EDGE_CURVE('',#1575,#1574,#272,.T.);
#1974=EDGE_CURVE('',#1576,#1575,#273,.T.);
#1975=EDGE_CURVE('',#1574,#1576,#274,.T.);
#1976=EDGE_CURVE('',#1577,#1578,#275,.T.);
#1977=EDGE_CURVE('',#1578,#1577,#276,.T.);
#1978=EDGE_CURVE('',#1578,#1579,#1014,.T.);
#1979=EDGE_CURVE('',#1580,#1579,#277,.T.);
#1980=EDGE_CURVE('',#1579,#1580,#278,.T.);
#1981=EDGE_CURVE('',#1581,#1582,#279,.T.);
#1982=EDGE_CURVE('',#1583,#1581,#280,.T.);
#1983=EDGE_CURVE('',#1582,#1583,#281,.T.);
#1984=EDGE_CURVE('',#1582,#1584,#1015,.T.);
#1985=EDGE_CURVE('',#1585,#1584,#282,.T.);
#1986=EDGE_CURVE('',#1586,#1585,#283,.T.);
#1987=EDGE_CURVE('',#1584,#1586,#284,.T.);
#1988=EDGE_CURVE('',#1587,#1588,#285,.T.);
#1989=EDGE_CURVE('',#1588,#1587,#286,.T.);
#1990=EDGE_CURVE('',#1588,#1589,#1016,.T.);
#1991=EDGE_CURVE('',#1590,#1589,#287,.T.);
#1992=EDGE_CURVE('',#1589,#1590,#288,.T.);
#1993=EDGE_CURVE('',#1591,#1592,#289,.T.);
#1994=EDGE_CURVE('',#1593,#1591,#290,.T.);
#1995=EDGE_CURVE('',#1592,#1593,#291,.T.);
#1996=EDGE_CURVE('',#1592,#1594,#1017,.T.);
#1997=EDGE_CURVE('',#1595,#1594,#292,.T.);
#1998=EDGE_CURVE('',#1596,#1595,#293,.T.);
#1999=EDGE_CURVE('',#1594,#1596,#294,.T.);
#2000=EDGE_CURVE('',#1597,#1598,#295,.T.);
#2001=EDGE_CURVE('',#1598,#1597,#296,.T.);
#2002=EDGE_CURVE('',#1598,#1599,#1018,.T.);
#2003=EDGE_CURVE('',#1600,#1599,#297,.T.);
#2004=EDGE_CURVE('',#1599,#1600,#298,.T.);
#2005=EDGE_CURVE('',#1601,#1602,#299,.T.);
#2006=EDGE_CURVE('',#1603,#1601,#300,.T.);
#2007=EDGE_CURVE('',#1602,#1603,#301,.T.);
#2008=EDGE_CURVE('',#1602,#1604,#1019,.T.);
#2009=EDGE_CURVE('',#1605,#1604,#302,.T.);
#2010=EDGE_CURVE('',#1606,#1605,#303,.T.);
#2011=EDGE_CURVE('',#1604,#1606,#304,.T.);
#2012=EDGE_CURVE('',#1607,#1608,#305,.T.);
#2013=EDGE_CURVE('',#1608,#1607,#306,.T.);
#2014=EDGE_CURVE('',#1608,#1609,#1020,.T.);
#2015=EDGE_CURVE('',#1610,#1609,#307,.T.);
#2016=EDGE_CURVE('',#1609,#1610,#308,.T.);
#2017=EDGE_CURVE('',#1611,#1612,#309,.T.);
#2018=EDGE_CURVE('',#1613,#1611,#310,.T.);
#2019=EDGE_CURVE('',#1612,#1613,#311,.T.);
#2020=EDGE_CURVE('',#1612,#1614,#1021,.T.);
#2021=EDGE_CURVE('',#1615,#1614,#312,.T.);
#2022=EDGE_CURVE('',#1616,#1615,#313,.T.);
#2023=EDGE_CURVE('',#1614,#1616,#314,.T.);
#2024=EDGE_CURVE('',#1617,#1618,#315,.T.);
#2025=EDGE_CURVE('',#1618,#1617,#316,.T.);
#2026=EDGE_CURVE('',#1618,#1619,#1022,.T.);
#2027=EDGE_CURVE('',#1620,#1619,#317,.T.);
#2028=EDGE_CURVE('',#1619,#1620,#318,.T.);
#2029=EDGE_CURVE('',#1621,#1621,#1315,.T.);
#2030=EDGE_CURVE('',#1621,#1622,#1023,.T.);
#2031=EDGE_CURVE('',#1622,#1622,#1316,.T.);
#2032=EDGE_CURVE('',#1623,#1623,#1317,.T.);
#2033=EDGE_CURVE('',#1623,#1605,#1024,.T.);
#2034=EDGE_CURVE('',#1604,#1595,#1025,.T.);
#2035=EDGE_CURVE('',#1594,#1585,#1026,.T.);
#2036=EDGE_CURVE('',#1584,#1575,#1027,.T.);
#2037=EDGE_CURVE('',#1574,#1615,#1028,.T.);
#2038=EDGE_CURVE('',#1614,#1565,#1029,.T.);
#2039=EDGE_CURVE('',#1564,#1624,#1030,.T.);
#2040=EDGE_CURVE('',#1624,#1624,#1318,.T.);
#2041=EDGE_CURVE('',#1625,#1625,#1319,.T.);
#2042=EDGE_CURVE('',#1626,#1626,#1320,.T.);
#2043=EDGE_CURVE('',#1626,#1625,#1031,.T.);
#2044=EDGE_CURVE('',#1627,#1627,#1321,.T.);
#2045=EDGE_CURVE('',#1627,#1562,#1032,.T.);
#2046=EDGE_CURVE('',#1563,#1612,#1033,.T.);
#2047=EDGE_CURVE('',#1613,#1572,#1034,.T.);
#2048=EDGE_CURVE('',#1573,#1582,#1035,.T.);
#2049=EDGE_CURVE('',#1583,#1592,#1036,.T.);
#2050=EDGE_CURVE('',#1593,#1602,#1037,.T.);
#2051=EDGE_CURVE('',#1603,#1628,#1038,.T.);
#2052=EDGE_CURVE('',#1628,#1628,#1322,.T.);
#2053=EDGE_CURVE('',#1629,#1629,#1323,.T.);
#2054=EDGE_CURVE('',#1630,#1630,#1324,.T.);
#2055=EDGE_CURVE('',#1631,#1631,#1325,.T.);
#2056=EDGE_CURVE('',#1631,#1629,#1039,.T.);
#2057=EDGE_CURVE('',#1630,#1632,#1040,.T.);
#2058=EDGE_CURVE('',#1632,#1632,#1326,.T.);
#2059=EDGE_CURVE('',#1633,#1633,#1327,.T.);
#2060=EDGE_CURVE('',#1633,#1634,#1041,.T.);
#2061=EDGE_CURVE('',#1634,#1634,#1328,.T.);
#2062=EDGE_CURVE('',#1635,#1635,#1329,.T.);
#2063=EDGE_CURVE('',#1635,#1636,#1042,.T.);
#2064=EDGE_CURVE('',#1636,#1636,#1330,.T.);
#2065=EDGE_CURVE('',#1637,#1637,#1331,.T.);
#2066=EDGE_CURVE('',#1637,#1638,#1043,.T.);
#2067=EDGE_CURVE('',#1638,#1638,#1332,.T.);
#2068=EDGE_CURVE('',#1639,#1639,#1333,.T.);
#2069=EDGE_CURVE('',#1639,#1640,#1044,.T.);
#2070=EDGE_CURVE('',#1640,#1640,#1334,.T.);
#2071=EDGE_CURVE('',#1641,#1641,#1335,.T.);
#2072=EDGE_CURVE('',#1641,#1642,#1045,.T.);
#2073=EDGE_CURVE('',#1642,#1642,#1336,.T.);
#2074=EDGE_CURVE('',#1643,#1643,#1337,.T.);
#2075=EDGE_CURVE('',#1643,#1644,#1046,.T.);
#2076=EDGE_CURVE('',#1644,#1644,#1338,.T.);
#2077=EDGE_CURVE('',#1645,#1645,#1339,.T.);
#2078=EDGE_CURVE('',#1645,#1646,#1047,.T.);
#2079=EDGE_CURVE('',#1646,#1646,#1340,.T.);
#2080=EDGE_CURVE('',#1647,#1647,#1341,.T.);
#2081=EDGE_CURVE('',#1647,#1648,#1048,.T.);
#2082=EDGE_CURVE('',#1648,#1648,#1342,.T.);
#2083=EDGE_CURVE('',#1649,#1649,#1343,.T.);
#2084=EDGE_CURVE('',#1649,#1650,#1049,.T.);
#2085=EDGE_CURVE('',#1650,#1650,#1344,.T.);
#2086=EDGE_CURVE('',#1651,#1651,#1345,.T.);
#2087=EDGE_CURVE('',#1651,#1652,#1050,.T.);
#2088=EDGE_CURVE('',#1652,#1652,#1346,.T.);
#2089=EDGE_CURVE('',#1653,#1653,#1347,.T.);
#2090=EDGE_CURVE('',#1653,#1654,#1051,.T.);
#2091=EDGE_CURVE('',#1654,#1654,#1348,.T.);
#2092=EDGE_CURVE('',#1655,#1655,#1349,.T.);
#2093=EDGE_CURVE('',#1655,#1656,#1052,.T.);
#2094=EDGE_CURVE('',#1656,#1656,#1350,.T.);
#2095=EDGE_CURVE('',#1657,#1657,#1351,.T.);
#2096=EDGE_CURVE('',#1657,#1658,#1053,.T.);
#2097=EDGE_CURVE('',#1658,#1658,#1352,.T.);
#2098=EDGE_CURVE('',#1659,#1659,#1353,.T.);
#2099=EDGE_CURVE('',#1659,#1660,#1054,.T.);
#2100=EDGE_CURVE('',#1660,#1660,#1354,.T.);
#2101=EDGE_CURVE('',#1661,#1661,#1355,.T.);
#2102=EDGE_CURVE('',#1661,#1662,#1055,.T.);
#2103=EDGE_CURVE('',#1662,#1662,#1356,.T.);
#2104=EDGE_CURVE('',#1663,#1663,#1357,.T.);
#2105=EDGE_CURVE('',#1663,#1664,#1056,.T.);
#2106=EDGE_CURVE('',#1664,#1664,#1358,.T.);
#2107=EDGE_CURVE('',#1665,#1665,#1359,.T.);
#2108=EDGE_CURVE('',#1665,#1666,#1057,.T.);
#2109=EDGE_CURVE('',#1666,#1666,#1360,.T.);
#2110=EDGE_CURVE('',#1667,#1667,#1361,.T.);
#2111=EDGE_CURVE('',#1668,#1668,#1362,.T.);
#2112=EDGE_CURVE('',#1668,#1667,#1058,.T.);
#2113=EDGE_CURVE('',#1669,#1669,#1363,.T.);
#2114=EDGE_CURVE('',#1669,#1668,#1059,.T.);
#2115=EDGE_CURVE('',#1670,#1670,#1364,.T.);
#2116=EDGE_CURVE('',#1670,#1669,#1060,.T.);
#2117=EDGE_CURVE('',#1671,#1671,#1365,.T.);
#2118=EDGE_CURVE('',#1672,#1672,#1366,.F.);
#2119=EDGE_CURVE('',#1672,#1671,#1061,.T.);
#2120=EDGE_CURVE('',#1673,#1673,#1367,.F.);
#2121=EDGE_CURVE('',#1673,#1672,#1062,.T.);
#2122=EDGE_CURVE('',#1674,#1674,#1368,.T.);
#2123=EDGE_CURVE('',#1674,#1673,#1063,.T.);
#2124=EDGE_CURVE('',#1675,#1676,#1064,.T.);
#2125=EDGE_CURVE('',#1676,#1677,#1065,.T.);
#2126=EDGE_CURVE('',#1677,#1678,#1066,.T.);
#2127=EDGE_CURVE('',#1675,#1678,#1067,.T.);
#2128=EDGE_CURVE('',#1676,#1679,#1068,.T.);
#2129=EDGE_CURVE('',#1679,#1680,#1069,.T.);
#2130=EDGE_CURVE('',#1680,#1677,#1070,.T.);
#2131=EDGE_CURVE('',#1679,#1681,#1071,.T.);
#2132=EDGE_CURVE('',#1681,#1682,#1072,.T.);
#2133=EDGE_CURVE('',#1682,#1680,#1073,.T.);
#2134=EDGE_CURVE('',#1681,#1683,#1074,.T.);
#2135=EDGE_CURVE('',#1683,#1684,#1075,.T.);
#2136=EDGE_CURVE('',#1684,#1682,#1076,.T.);
#2137=EDGE_CURVE('',#1683,#1685,#1077,.T.);
#2138=EDGE_CURVE('',#1685,#1686,#1078,.T.);
#2139=EDGE_CURVE('',#1686,#1684,#1079,.T.);
#2140=EDGE_CURVE('',#1685,#1675,#1080,.T.);
#2141=EDGE_CURVE('',#1678,#1686,#1081,.T.);
#2142=EDGE_CURVE('',#1687,#1688,#1082,.T.);
#2143=EDGE_CURVE('',#1688,#1689,#1083,.T.);
#2144=EDGE_CURVE('',#1689,#1690,#1084,.T.);
#2145=EDGE_CURVE('',#1690,#1691,#1085,.T.);
#2146=EDGE_CURVE('',#1691,#1692,#1086,.T.);
#2147=EDGE_CURVE('',#1692,#1687,#1087,.T.);
#2148=EDGE_CURVE('',#1693,#1693,#1369,.T.);
#2149=EDGE_CURVE('',#1694,#1695,#1088,.T.);
#2150=EDGE_CURVE('',#1695,#1696,#1089,.T.);
#2151=EDGE_CURVE('',#1696,#1697,#1090,.T.);
#2152=EDGE_CURVE('',#1697,#1698,#1091,.T.);
#2153=EDGE_CURVE('',#1698,#1699,#1092,.T.);
#2154=EDGE_CURVE('',#1699,#1694,#1093,.T.);
#2155=EDGE_CURVE('',#1700,#1700,#1370,.T.);
#2156=EDGE_CURVE('',#1694,#1688,#1094,.T.);
#2157=EDGE_CURVE('',#1689,#1699,#1095,.T.);
#2158=EDGE_CURVE('',#1690,#1698,#1096,.T.);
#2159=EDGE_CURVE('',#1691,#1697,#1097,.T.);
#2160=EDGE_CURVE('',#1692,#1696,#1098,.T.);
#2161=EDGE_CURVE('',#1687,#1695,#1099,.T.);
#2162=EDGE_CURVE('',#1700,#1701,#1100,.T.);
#2163=EDGE_CURVE('',#1701,#1701,#1371,.T.);
#2164=EDGE_CURVE('',#1702,#1702,#1372,.T.);
#2165=EDGE_CURVE('',#1703,#1703,#1373,.T.);
#2166=EDGE_CURVE('',#1701,#1702,#1101,.T.);
#2167=EDGE_CURVE('',#1704,#1704,#1374,.T.);
#2168=EDGE_CURVE('',#1704,#1693,#1102,.T.);
#2169=EDGE_CURVE('',#1705,#1705,#1375,.T.);
#2170=EDGE_CURVE('',#1705,#1704,#1103,.T.);
#2171=EDGE_CURVE('',#1706,#1706,#1376,.T.);
#2172=EDGE_CURVE('',#1706,#1703,#1104,.T.);
#2173=EDGE_CURVE('',#1707,#1708,#1105,.T.);
#2174=EDGE_CURVE('',#1709,#1707,#1106,.T.);
#2175=EDGE_CURVE('',#1710,#1709,#1107,.T.);
#2176=EDGE_CURVE('',#1711,#1710,#1108,.T.);
#2177=EDGE_CURVE('',#1712,#1711,#1109,.T.);
#2178=EDGE_CURVE('',#1708,#1712,#1110,.T.);
#2179=EDGE_CURVE('',#1713,#1713,#1377,.T.);
#2180=EDGE_CURVE('',#1707,#1714,#1111,.T.);
#2181=EDGE_CURVE('',#1715,#1714,#1112,.T.);
#2182=EDGE_CURVE('',#1709,#1715,#1113,.T.);
#2183=EDGE_CURVE('',#1716,#1715,#1114,.T.);
#2184=EDGE_CURVE('',#1710,#1716,#1115,.T.);
#2185=EDGE_CURVE('',#1717,#1716,#1116,.T.);
#2186=EDGE_CURVE('',#1711,#1717,#1117,.T.);
#2187=EDGE_CURVE('',#1718,#1717,#1118,.T.);
#2188=EDGE_CURVE('',#1712,#1718,#1119,.T.);
#2189=EDGE_CURVE('',#1719,#1718,#1120,.T.);
#2190=EDGE_CURVE('',#1708,#1719,#1121,.T.);
#2191=EDGE_CURVE('',#1714,#1719,#1122,.T.);
#2192=EDGE_CURVE('',#1713,#1720,#1123,.T.);
#2193=EDGE_CURVE('',#1720,#1720,#1378,.T.);
#2194=ORIENTED_EDGE('',*,*,#1721,.F.);
#2195=ORIENTED_EDGE('',*,*,#1722,.T.);
#2196=ORIENTED_EDGE('',*,*,#1723,.F.);
#2197=ORIENTED_EDGE('',*,*,#1722,.F.);
#2198=ORIENTED_EDGE('',*,*,#1724,.F.);
#2199=ORIENTED_EDGE('',*,*,#1725,.T.);
#2200=ORIENTED_EDGE('',*,*,#1726,.F.);
#2201=ORIENTED_EDGE('',*,*,#1725,.F.);
#2202=ORIENTED_EDGE('',*,*,#1727,.F.);
#2203=ORIENTED_EDGE('',*,*,#1728,.T.);
#2204=ORIENTED_EDGE('',*,*,#1729,.F.);
#2205=ORIENTED_EDGE('',*,*,#1728,.F.);
#2206=ORIENTED_EDGE('',*,*,#1730,.F.);
#2207=ORIENTED_EDGE('',*,*,#1731,.T.);
#2208=ORIENTED_EDGE('',*,*,#1732,.F.);
#2209=ORIENTED_EDGE('',*,*,#1731,.F.);
#2210=ORIENTED_EDGE('',*,*,#1733,.F.);
#2211=ORIENTED_EDGE('',*,*,#1734,.T.);
#2212=ORIENTED_EDGE('',*,*,#1735,.F.);
#2213=ORIENTED_EDGE('',*,*,#1736,.F.);
#2214=ORIENTED_EDGE('',*,*,#1737,.F.);
#2215=ORIENTED_EDGE('',*,*,#1738,.F.);
#2216=ORIENTED_EDGE('',*,*,#1734,.F.);
#2217=ORIENTED_EDGE('',*,*,#1739,.F.);
#2218=ORIENTED_EDGE('',*,*,#1740,.T.);
#2219=ORIENTED_EDGE('',*,*,#1741,.F.);
#2220=ORIENTED_EDGE('',*,*,#1740,.F.);
#2221=ORIENTED_EDGE('',*,*,#1736,.T.);
#2222=ORIENTED_EDGE('',*,*,#1742,.T.);
#2223=ORIENTED_EDGE('',*,*,#1743,.T.);
#2224=ORIENTED_EDGE('',*,*,#1744,.F.);
#2225=ORIENTED_EDGE('',*,*,#1745,.F.);
#2226=ORIENTED_EDGE('',*,*,#1746,.T.);
#2227=ORIENTED_EDGE('',*,*,#1737,.T.);
#2228=ORIENTED_EDGE('',*,*,#1746,.F.);
#2229=ORIENTED_EDGE('',*,*,#1747,.F.);
#2230=ORIENTED_EDGE('',*,*,#1748,.F.);
#2231=ORIENTED_EDGE('',*,*,#1749,.F.);
#2232=ORIENTED_EDGE('',*,*,#1750,.F.);
#2233=ORIENTED_EDGE('',*,*,#1747,.T.);
#2234=ORIENTED_EDGE('',*,*,#1745,.T.);
#2235=ORIENTED_EDGE('',*,*,#1751,.T.);
#2236=ORIENTED_EDGE('',*,*,#1752,.T.);
#2237=ORIENTED_EDGE('',*,*,#1753,.T.);
#2238=ORIENTED_EDGE('',*,*,#1754,.T.);
#2239=ORIENTED_EDGE('',*,*,#1748,.T.);
#2240=ORIENTED_EDGE('',*,*,#1744,.T.);
#2241=ORIENTED_EDGE('',*,*,#1750,.T.);
#2242=ORIENTED_EDGE('',*,*,#1755,.T.);
#2243=ORIENTED_EDGE('',*,*,#1756,.T.);
#2244=ORIENTED_EDGE('',*,*,#1752,.F.);
#2245=ORIENTED_EDGE('',*,*,#1756,.F.);
#2246=ORIENTED_EDGE('',*,*,#1757,.T.);
#2247=ORIENTED_EDGE('',*,*,#1753,.F.);
#2248=ORIENTED_EDGE('',*,*,#1755,.F.);
#2249=ORIENTED_EDGE('',*,*,#1749,.T.);
#2250=ORIENTED_EDGE('',*,*,#1754,.F.);
#2251=ORIENTED_EDGE('',*,*,#1757,.F.);
#2252=ORIENTED_EDGE('',*,*,#1758,.F.);
#2253=ORIENTED_EDGE('',*,*,#1759,.T.);
#2254=ORIENTED_EDGE('',*,*,#1760,.F.);
#2255=ORIENTED_EDGE('',*,*,#1759,.F.);
#2256=ORIENTED_EDGE('',*,*,#1758,.T.);
#2257=ORIENTED_EDGE('',*,*,#1761,.F.);
#2258=ORIENTED_EDGE('',*,*,#1762,.F.);
#2259=ORIENTED_EDGE('',*,*,#1763,.T.);
#2260=ORIENTED_EDGE('',*,*,#1764,.T.);
#2261=ORIENTED_EDGE('',*,*,#1763,.F.);
#2262=ORIENTED_EDGE('',*,*,#1764,.F.);
#2263=ORIENTED_EDGE('',*,*,#1751,.F.);
#2264=ORIENTED_EDGE('',*,*,#1733,.T.);
#2265=ORIENTED_EDGE('',*,*,#1743,.F.);
#2266=ORIENTED_EDGE('',*,*,#1765,.T.);
#2267=ORIENTED_EDGE('',*,*,#1761,.T.);
#2268=ORIENTED_EDGE('',*,*,#1765,.F.);
#2269=ORIENTED_EDGE('',*,*,#1742,.F.);
#2270=ORIENTED_EDGE('',*,*,#1735,.T.);
#2271=ORIENTED_EDGE('',*,*,#1738,.T.);
#2272=ORIENTED_EDGE('',*,*,#1739,.T.);
#2273=ORIENTED_EDGE('',*,*,#1766,.F.);
#2274=ORIENTED_EDGE('',*,*,#1721,.T.);
#2275=ORIENTED_EDGE('',*,*,#1724,.T.);
#2276=ORIENTED_EDGE('',*,*,#1727,.T.);
#2277=ORIENTED_EDGE('',*,*,#1730,.T.);
#2278=ORIENTED_EDGE('',*,*,#1767,.F.);
#2279=ORIENTED_EDGE('',*,*,#1768,.F.);
#2280=ORIENTED_EDGE('',*,*,#1769,.T.);
#2281=ORIENTED_EDGE('',*,*,#1766,.T.);
#2282=ORIENTED_EDGE('',*,*,#1769,.F.);
#2283=ORIENTED_EDGE('',*,*,#1767,.T.);
#2284=ORIENTED_EDGE('',*,*,#1770,.T.);
#2285=ORIENTED_EDGE('',*,*,#1771,.F.);
#2286=ORIENTED_EDGE('',*,*,#1772,.F.);
#2287=ORIENTED_EDGE('',*,*,#1773,.F.);
#2288=ORIENTED_EDGE('',*,*,#1770,.F.);
#2289=ORIENTED_EDGE('',*,*,#1768,.T.);
#2290=ORIENTED_EDGE('',*,*,#1723,.T.);
#2291=ORIENTED_EDGE('',*,*,#1726,.T.);
#2292=ORIENTED_EDGE('',*,*,#1729,.T.);
#2293=ORIENTED_EDGE('',*,*,#1732,.T.);
#2294=ORIENTED_EDGE('',*,*,#1741,.T.);
#2295=ORIENTED_EDGE('',*,*,#1774,.F.);
#2296=ORIENTED_EDGE('',*,*,#1775,.T.);
#2297=ORIENTED_EDGE('',*,*,#1776,.T.);
#2298=ORIENTED_EDGE('',*,*,#1775,.F.);
#2299=ORIENTED_EDGE('',*,*,#1771,.T.);
#2300=ORIENTED_EDGE('',*,*,#1773,.T.);
#2301=ORIENTED_EDGE('',*,*,#1772,.T.);
#2302=ORIENTED_EDGE('',*,*,#1774,.T.);
#2303=ORIENTED_EDGE('',*,*,#1760,.T.);
#2304=ORIENTED_EDGE('',*,*,#1776,.F.);
#2305=ORIENTED_EDGE('',*,*,#1762,.T.);
#2306=ORIENTED_EDGE('',*,*,#1777,.F.);
#2307=ORIENTED_EDGE('',*,*,#1778,.F.);
#2308=ORIENTED_EDGE('',*,*,#1779,.T.);
#2309=ORIENTED_EDGE('',*,*,#1780,.F.);
#2310=ORIENTED_EDGE('',*,*,#1781,.F.);
#2311=ORIENTED_EDGE('',*,*,#1779,.F.);
#2312=ORIENTED_EDGE('',*,*,#1782,.F.);
#2313=ORIENTED_EDGE('',*,*,#1783,.F.);
#2314=ORIENTED_EDGE('',*,*,#1784,.T.);
#2315=ORIENTED_EDGE('',*,*,#1785,.F.);
#2316=ORIENTED_EDGE('',*,*,#1786,.F.);
#2317=ORIENTED_EDGE('',*,*,#1784,.F.);
#2318=ORIENTED_EDGE('',*,*,#1787,.F.);
#2319=ORIENTED_EDGE('',*,*,#1788,.F.);
#2320=ORIENTED_EDGE('',*,*,#1789,.T.);
#2321=ORIENTED_EDGE('',*,*,#1790,.F.);
#2322=ORIENTED_EDGE('',*,*,#1791,.F.);
#2323=ORIENTED_EDGE('',*,*,#1789,.F.);
#2324=ORIENTED_EDGE('',*,*,#1792,.F.);
#2325=ORIENTED_EDGE('',*,*,#1793,.F.);
#2326=ORIENTED_EDGE('',*,*,#1794,.T.);
#2327=ORIENTED_EDGE('',*,*,#1795,.F.);
#2328=ORIENTED_EDGE('',*,*,#1796,.F.);
#2329=ORIENTED_EDGE('',*,*,#1794,.F.);
#2330=ORIENTED_EDGE('',*,*,#1797,.F.);
#2331=ORIENTED_EDGE('',*,*,#1798,.F.);
#2332=ORIENTED_EDGE('',*,*,#1799,.T.);
#2333=ORIENTED_EDGE('',*,*,#1800,.F.);
#2334=ORIENTED_EDGE('',*,*,#1801,.F.);
#2335=ORIENTED_EDGE('',*,*,#1799,.F.);
#2336=ORIENTED_EDGE('',*,*,#1802,.F.);
#2337=ORIENTED_EDGE('',*,*,#1803,.F.);
#2338=ORIENTED_EDGE('',*,*,#1804,.T.);
#2339=ORIENTED_EDGE('',*,*,#1805,.F.);
#2340=ORIENTED_EDGE('',*,*,#1806,.F.);
#2341=ORIENTED_EDGE('',*,*,#1804,.F.);
#2342=ORIENTED_EDGE('',*,*,#1807,.F.);
#2343=ORIENTED_EDGE('',*,*,#1808,.F.);
#2344=ORIENTED_EDGE('',*,*,#1809,.T.);
#2345=ORIENTED_EDGE('',*,*,#1810,.F.);
#2346=ORIENTED_EDGE('',*,*,#1811,.F.);
#2347=ORIENTED_EDGE('',*,*,#1809,.F.);
#2348=ORIENTED_EDGE('',*,*,#1812,.F.);
#2349=ORIENTED_EDGE('',*,*,#1813,.F.);
#2350=ORIENTED_EDGE('',*,*,#1814,.T.);
#2351=ORIENTED_EDGE('',*,*,#1815,.F.);
#2352=ORIENTED_EDGE('',*,*,#1816,.F.);
#2353=ORIENTED_EDGE('',*,*,#1814,.F.);
#2354=ORIENTED_EDGE('',*,*,#1817,.F.);
#2355=ORIENTED_EDGE('',*,*,#1818,.F.);
#2356=ORIENTED_EDGE('',*,*,#1819,.T.);
#2357=ORIENTED_EDGE('',*,*,#1820,.F.);
#2358=ORIENTED_EDGE('',*,*,#1821,.F.);
#2359=ORIENTED_EDGE('',*,*,#1819,.F.);
#2360=ORIENTED_EDGE('',*,*,#1822,.F.);
#2361=ORIENTED_EDGE('',*,*,#1823,.F.);
#2362=ORIENTED_EDGE('',*,*,#1824,.T.);
#2363=ORIENTED_EDGE('',*,*,#1825,.F.);
#2364=ORIENTED_EDGE('',*,*,#1826,.F.);
#2365=ORIENTED_EDGE('',*,*,#1824,.F.);
#2366=ORIENTED_EDGE('',*,*,#1827,.F.);
#2367=ORIENTED_EDGE('',*,*,#1828,.F.);
#2368=ORIENTED_EDGE('',*,*,#1829,.T.);
#2369=ORIENTED_EDGE('',*,*,#1830,.F.);
#2370=ORIENTED_EDGE('',*,*,#1831,.F.);
#2371=ORIENTED_EDGE('',*,*,#1829,.F.);
#2372=ORIENTED_EDGE('',*,*,#1832,.F.);
#2373=ORIENTED_EDGE('',*,*,#1833,.F.);
#2374=ORIENTED_EDGE('',*,*,#1834,.T.);
#2375=ORIENTED_EDGE('',*,*,#1835,.F.);
#2376=ORIENTED_EDGE('',*,*,#1836,.F.);
#2377=ORIENTED_EDGE('',*,*,#1834,.F.);
#2378=ORIENTED_EDGE('',*,*,#1837,.F.);
#2379=ORIENTED_EDGE('',*,*,#1838,.F.);
#2380=ORIENTED_EDGE('',*,*,#1839,.T.);
#2381=ORIENTED_EDGE('',*,*,#1840,.F.);
#2382=ORIENTED_EDGE('',*,*,#1841,.F.);
#2383=ORIENTED_EDGE('',*,*,#1839,.F.);
#2384=ORIENTED_EDGE('',*,*,#1842,.F.);
#2385=ORIENTED_EDGE('',*,*,#1843,.F.);
#2386=ORIENTED_EDGE('',*,*,#1844,.T.);
#2387=ORIENTED_EDGE('',*,*,#1845,.F.);
#2388=ORIENTED_EDGE('',*,*,#1846,.F.);
#2389=ORIENTED_EDGE('',*,*,#1844,.F.);
#2390=ORIENTED_EDGE('',*,*,#1847,.F.);
#2391=ORIENTED_EDGE('',*,*,#1848,.F.);
#2392=ORIENTED_EDGE('',*,*,#1849,.T.);
#2393=ORIENTED_EDGE('',*,*,#1850,.F.);
#2394=ORIENTED_EDGE('',*,*,#1851,.F.);
#2395=ORIENTED_EDGE('',*,*,#1849,.F.);
#2396=ORIENTED_EDGE('',*,*,#1852,.F.);
#2397=ORIENTED_EDGE('',*,*,#1853,.F.);
#2398=ORIENTED_EDGE('',*,*,#1854,.T.);
#2399=ORIENTED_EDGE('',*,*,#1855,.F.);
#2400=ORIENTED_EDGE('',*,*,#1856,.F.);
#2401=ORIENTED_EDGE('',*,*,#1854,.F.);
#2402=ORIENTED_EDGE('',*,*,#1857,.F.);
#2403=ORIENTED_EDGE('',*,*,#1858,.F.);
#2404=ORIENTED_EDGE('',*,*,#1859,.T.);
#2405=ORIENTED_EDGE('',*,*,#1860,.F.);
#2406=ORIENTED_EDGE('',*,*,#1861,.F.);
#2407=ORIENTED_EDGE('',*,*,#1859,.F.);
#2408=ORIENTED_EDGE('',*,*,#1862,.F.);
#2409=ORIENTED_EDGE('',*,*,#1863,.F.);
#2410=ORIENTED_EDGE('',*,*,#1864,.T.);
#2411=ORIENTED_EDGE('',*,*,#1865,.F.);
#2412=ORIENTED_EDGE('',*,*,#1866,.F.);
#2413=ORIENTED_EDGE('',*,*,#1864,.F.);
#2414=ORIENTED_EDGE('',*,*,#1867,.F.);
#2415=ORIENTED_EDGE('',*,*,#1868,.F.);
#2416=ORIENTED_EDGE('',*,*,#1869,.T.);
#2417=ORIENTED_EDGE('',*,*,#1870,.F.);
#2418=ORIENTED_EDGE('',*,*,#1871,.F.);
#2419=ORIENTED_EDGE('',*,*,#1869,.F.);
#2420=ORIENTED_EDGE('',*,*,#1872,.F.);
#2421=ORIENTED_EDGE('',*,*,#1873,.F.);
#2422=ORIENTED_EDGE('',*,*,#1874,.T.);
#2423=ORIENTED_EDGE('',*,*,#1875,.F.);
#2424=ORIENTED_EDGE('',*,*,#1876,.F.);
#2425=ORIENTED_EDGE('',*,*,#1874,.F.);
#2426=ORIENTED_EDGE('',*,*,#1877,.F.);
#2427=ORIENTED_EDGE('',*,*,#1878,.F.);
#2428=ORIENTED_EDGE('',*,*,#1879,.T.);
#2429=ORIENTED_EDGE('',*,*,#1880,.F.);
#2430=ORIENTED_EDGE('',*,*,#1881,.F.);
#2431=ORIENTED_EDGE('',*,*,#1879,.F.);
#2432=ORIENTED_EDGE('',*,*,#1882,.F.);
#2433=ORIENTED_EDGE('',*,*,#1883,.F.);
#2434=ORIENTED_EDGE('',*,*,#1884,.T.);
#2435=ORIENTED_EDGE('',*,*,#1885,.F.);
#2436=ORIENTED_EDGE('',*,*,#1886,.F.);
#2437=ORIENTED_EDGE('',*,*,#1884,.F.);
#2438=ORIENTED_EDGE('',*,*,#1887,.F.);
#2439=ORIENTED_EDGE('',*,*,#1888,.F.);
#2440=ORIENTED_EDGE('',*,*,#1889,.T.);
#2441=ORIENTED_EDGE('',*,*,#1890,.F.);
#2442=ORIENTED_EDGE('',*,*,#1891,.F.);
#2443=ORIENTED_EDGE('',*,*,#1889,.F.);
#2444=ORIENTED_EDGE('',*,*,#1892,.F.);
#2445=ORIENTED_EDGE('',*,*,#1893,.F.);
#2446=ORIENTED_EDGE('',*,*,#1894,.T.);
#2447=ORIENTED_EDGE('',*,*,#1895,.F.);
#2448=ORIENTED_EDGE('',*,*,#1896,.F.);
#2449=ORIENTED_EDGE('',*,*,#1894,.F.);
#2450=ORIENTED_EDGE('',*,*,#1897,.F.);
#2451=ORIENTED_EDGE('',*,*,#1898,.F.);
#2452=ORIENTED_EDGE('',*,*,#1899,.T.);
#2453=ORIENTED_EDGE('',*,*,#1900,.F.);
#2454=ORIENTED_EDGE('',*,*,#1901,.F.);
#2455=ORIENTED_EDGE('',*,*,#1899,.F.);
#2456=ORIENTED_EDGE('',*,*,#1902,.F.);
#2457=ORIENTED_EDGE('',*,*,#1903,.F.);
#2458=ORIENTED_EDGE('',*,*,#1904,.T.);
#2459=ORIENTED_EDGE('',*,*,#1905,.F.);
#2460=ORIENTED_EDGE('',*,*,#1906,.F.);
#2461=ORIENTED_EDGE('',*,*,#1904,.F.);
#2462=ORIENTED_EDGE('',*,*,#1907,.F.);
#2463=ORIENTED_EDGE('',*,*,#1908,.F.);
#2464=ORIENTED_EDGE('',*,*,#1909,.T.);
#2465=ORIENTED_EDGE('',*,*,#1910,.F.);
#2466=ORIENTED_EDGE('',*,*,#1911,.F.);
#2467=ORIENTED_EDGE('',*,*,#1909,.F.);
#2468=ORIENTED_EDGE('',*,*,#1912,.F.);
#2469=ORIENTED_EDGE('',*,*,#1913,.F.);
#2470=ORIENTED_EDGE('',*,*,#1914,.T.);
#2471=ORIENTED_EDGE('',*,*,#1915,.F.);
#2472=ORIENTED_EDGE('',*,*,#1916,.F.);
#2473=ORIENTED_EDGE('',*,*,#1914,.F.);
#2474=ORIENTED_EDGE('',*,*,#1917,.F.);
#2475=ORIENTED_EDGE('',*,*,#1918,.F.);
#2476=ORIENTED_EDGE('',*,*,#1919,.T.);
#2477=ORIENTED_EDGE('',*,*,#1920,.F.);
#2478=ORIENTED_EDGE('',*,*,#1921,.F.);
#2479=ORIENTED_EDGE('',*,*,#1919,.F.);
#2480=ORIENTED_EDGE('',*,*,#1922,.F.);
#2481=ORIENTED_EDGE('',*,*,#1923,.F.);
#2482=ORIENTED_EDGE('',*,*,#1924,.T.);
#2483=ORIENTED_EDGE('',*,*,#1925,.F.);
#2484=ORIENTED_EDGE('',*,*,#1926,.F.);
#2485=ORIENTED_EDGE('',*,*,#1924,.F.);
#2486=ORIENTED_EDGE('',*,*,#1927,.F.);
#2487=ORIENTED_EDGE('',*,*,#1928,.F.);
#2488=ORIENTED_EDGE('',*,*,#1929,.T.);
#2489=ORIENTED_EDGE('',*,*,#1930,.F.);
#2490=ORIENTED_EDGE('',*,*,#1931,.F.);
#2491=ORIENTED_EDGE('',*,*,#1929,.F.);
#2492=ORIENTED_EDGE('',*,*,#1932,.F.);
#2493=ORIENTED_EDGE('',*,*,#1933,.F.);
#2494=ORIENTED_EDGE('',*,*,#1934,.T.);
#2495=ORIENTED_EDGE('',*,*,#1935,.F.);
#2496=ORIENTED_EDGE('',*,*,#1936,.F.);
#2497=ORIENTED_EDGE('',*,*,#1934,.F.);
#2498=ORIENTED_EDGE('',*,*,#1937,.F.);
#2499=ORIENTED_EDGE('',*,*,#1938,.F.);
#2500=ORIENTED_EDGE('',*,*,#1939,.T.);
#2501=ORIENTED_EDGE('',*,*,#1940,.F.);
#2502=ORIENTED_EDGE('',*,*,#1941,.F.);
#2503=ORIENTED_EDGE('',*,*,#1939,.F.);
#2504=ORIENTED_EDGE('',*,*,#1942,.F.);
#2505=ORIENTED_EDGE('',*,*,#1943,.F.);
#2506=ORIENTED_EDGE('',*,*,#1944,.T.);
#2507=ORIENTED_EDGE('',*,*,#1945,.F.);
#2508=ORIENTED_EDGE('',*,*,#1946,.F.);
#2509=ORIENTED_EDGE('',*,*,#1944,.F.);
#2510=ORIENTED_EDGE('',*,*,#1947,.F.);
#2511=ORIENTED_EDGE('',*,*,#1948,.F.);
#2512=ORIENTED_EDGE('',*,*,#1949,.T.);
#2513=ORIENTED_EDGE('',*,*,#1950,.F.);
#2514=ORIENTED_EDGE('',*,*,#1951,.F.);
#2515=ORIENTED_EDGE('',*,*,#1949,.F.);
#2516=ORIENTED_EDGE('',*,*,#1952,.F.);
#2517=ORIENTED_EDGE('',*,*,#1953,.F.);
#2518=ORIENTED_EDGE('',*,*,#1954,.T.);
#2519=ORIENTED_EDGE('',*,*,#1955,.F.);
#2520=ORIENTED_EDGE('',*,*,#1956,.F.);
#2521=ORIENTED_EDGE('',*,*,#1954,.F.);
#2522=ORIENTED_EDGE('',*,*,#1957,.F.);
#2523=ORIENTED_EDGE('',*,*,#1958,.F.);
#2524=ORIENTED_EDGE('',*,*,#1959,.F.);
#2525=ORIENTED_EDGE('',*,*,#1960,.T.);
#2526=ORIENTED_EDGE('',*,*,#1961,.F.);
#2527=ORIENTED_EDGE('',*,*,#1962,.F.);
#2528=ORIENTED_EDGE('',*,*,#1963,.F.);
#2529=ORIENTED_EDGE('',*,*,#1960,.F.);
#2530=ORIENTED_EDGE('',*,*,#1964,.F.);
#2531=ORIENTED_EDGE('',*,*,#1965,.F.);
#2532=ORIENTED_EDGE('',*,*,#1966,.T.);
#2533=ORIENTED_EDGE('',*,*,#1967,.F.);
#2534=ORIENTED_EDGE('',*,*,#1968,.F.);
#2535=ORIENTED_EDGE('',*,*,#1966,.F.);
#2536=ORIENTED_EDGE('',*,*,#1969,.F.);
#2537=ORIENTED_EDGE('',*,*,#1970,.F.);
#2538=ORIENTED_EDGE('',*,*,#1971,.F.);
#2539=ORIENTED_EDGE('',*,*,#1972,.T.);
#2540=ORIENTED_EDGE('',*,*,#1973,.F.);
#2541=ORIENTED_EDGE('',*,*,#1974,.F.);
#2542=ORIENTED_EDGE('',*,*,#1975,.F.);
#2543=ORIENTED_EDGE('',*,*,#1972,.F.);
#2544=ORIENTED_EDGE('',*,*,#1976,.F.);
#2545=ORIENTED_EDGE('',*,*,#1977,.F.);
#2546=ORIENTED_EDGE('',*,*,#1978,.T.);
#2547=ORIENTED_EDGE('',*,*,#1979,.F.);
#2548=ORIENTED_EDGE('',*,*,#1980,.F.);
#2549=ORIENTED_EDGE('',*,*,#1978,.F.);
#2550=ORIENTED_EDGE('',*,*,#1981,.F.);
#2551=ORIENTED_EDGE('',*,*,#1982,.F.);
#2552=ORIENTED_EDGE('',*,*,#1983,.F.);
#2553=ORIENTED_EDGE('',*,*,#1984,.T.);
#2554=ORIENTED_EDGE('',*,*,#1985,.F.);
#2555=ORIENTED_EDGE('',*,*,#1986,.F.);
#2556=ORIENTED_EDGE('',*,*,#1987,.F.);
#2557=ORIENTED_EDGE('',*,*,#1984,.F.);
#2558=ORIENTED_EDGE('',*,*,#1988,.F.);
#2559=ORIENTED_EDGE('',*,*,#1989,.F.);
#2560=ORIENTED_EDGE('',*,*,#1990,.T.);
#2561=ORIENTED_EDGE('',*,*,#1991,.F.);
#2562=ORIENTED_EDGE('',*,*,#1992,.F.);
#2563=ORIENTED_EDGE('',*,*,#1990,.F.);
#2564=ORIENTED_EDGE('',*,*,#1993,.F.);
#2565=ORIENTED_EDGE('',*,*,#1994,.F.);
#2566=ORIENTED_EDGE('',*,*,#1995,.F.);
#2567=ORIENTED_EDGE('',*,*,#1996,.T.);
#2568=ORIENTED_EDGE('',*,*,#1997,.F.);
#2569=ORIENTED_EDGE('',*,*,#1998,.F.);
#2570=ORIENTED_EDGE('',*,*,#1999,.F.);
#2571=ORIENTED_EDGE('',*,*,#1996,.F.);
#2572=ORIENTED_EDGE('',*,*,#2000,.F.);
#2573=ORIENTED_EDGE('',*,*,#2001,.F.);
#2574=ORIENTED_EDGE('',*,*,#2002,.T.);
#2575=ORIENTED_EDGE('',*,*,#2003,.F.);
#2576=ORIENTED_EDGE('',*,*,#2004,.F.);
#2577=ORIENTED_EDGE('',*,*,#2002,.F.);
#2578=ORIENTED_EDGE('',*,*,#2005,.F.);
#2579=ORIENTED_EDGE('',*,*,#2006,.F.);
#2580=ORIENTED_EDGE('',*,*,#2007,.F.);
#2581=ORIENTED_EDGE('',*,*,#2008,.T.);
#2582=ORIENTED_EDGE('',*,*,#2009,.F.);
#2583=ORIENTED_EDGE('',*,*,#2010,.F.);
#2584=ORIENTED_EDGE('',*,*,#2011,.F.);
#2585=ORIENTED_EDGE('',*,*,#2008,.F.);
#2586=ORIENTED_EDGE('',*,*,#2012,.F.);
#2587=ORIENTED_EDGE('',*,*,#2013,.F.);
#2588=ORIENTED_EDGE('',*,*,#2014,.T.);
#2589=ORIENTED_EDGE('',*,*,#2015,.F.);
#2590=ORIENTED_EDGE('',*,*,#2016,.F.);
#2591=ORIENTED_EDGE('',*,*,#2014,.F.);
#2592=ORIENTED_EDGE('',*,*,#2017,.F.);
#2593=ORIENTED_EDGE('',*,*,#2018,.F.);
#2594=ORIENTED_EDGE('',*,*,#2019,.F.);
#2595=ORIENTED_EDGE('',*,*,#2020,.T.);
#2596=ORIENTED_EDGE('',*,*,#2021,.F.);
#2597=ORIENTED_EDGE('',*,*,#2022,.F.);
#2598=ORIENTED_EDGE('',*,*,#2023,.F.);
#2599=ORIENTED_EDGE('',*,*,#2020,.F.);
#2600=ORIENTED_EDGE('',*,*,#2024,.F.);
#2601=ORIENTED_EDGE('',*,*,#2025,.F.);
#2602=ORIENTED_EDGE('',*,*,#2026,.T.);
#2603=ORIENTED_EDGE('',*,*,#2027,.F.);
#2604=ORIENTED_EDGE('',*,*,#2028,.F.);
#2605=ORIENTED_EDGE('',*,*,#2026,.F.);
#2606=ORIENTED_EDGE('',*,*,#2029,.F.);
#2607=ORIENTED_EDGE('',*,*,#2030,.T.);
#2608=ORIENTED_EDGE('',*,*,#2031,.F.);
#2609=ORIENTED_EDGE('',*,*,#2030,.F.);
#2610=ORIENTED_EDGE('',*,*,#2032,.F.);
#2611=ORIENTED_EDGE('',*,*,#2033,.T.);
#2612=ORIENTED_EDGE('',*,*,#2009,.T.);
#2613=ORIENTED_EDGE('',*,*,#2034,.T.);
#2614=ORIENTED_EDGE('',*,*,#1997,.T.);
#2615=ORIENTED_EDGE('',*,*,#2035,.T.);
#2616=ORIENTED_EDGE('',*,*,#1985,.T.);
#2617=ORIENTED_EDGE('',*,*,#2036,.T.);
#2618=ORIENTED_EDGE('',*,*,#1973,.T.);
#2619=ORIENTED_EDGE('',*,*,#2037,.T.);
#2620=ORIENTED_EDGE('',*,*,#2021,.T.);
#2621=ORIENTED_EDGE('',*,*,#2038,.T.);
#2622=ORIENTED_EDGE('',*,*,#1961,.T.);
#2623=ORIENTED_EDGE('',*,*,#2039,.T.);
#2624=ORIENTED_EDGE('',*,*,#2040,.T.);
#2625=ORIENTED_EDGE('',*,*,#2039,.F.);
#2626=ORIENTED_EDGE('',*,*,#1963,.T.);
#2627=ORIENTED_EDGE('',*,*,#1962,.T.);
#2628=ORIENTED_EDGE('',*,*,#2038,.F.);
#2629=ORIENTED_EDGE('',*,*,#2023,.T.);
#2630=ORIENTED_EDGE('',*,*,#2022,.T.);
#2631=ORIENTED_EDGE('',*,*,#2037,.F.);
#2632=ORIENTED_EDGE('',*,*,#1975,.T.);
#2633=ORIENTED_EDGE('',*,*,#1974,.T.);
#2634=ORIENTED_EDGE('',*,*,#2036,.F.);
#2635=ORIENTED_EDGE('',*,*,#1987,.T.);
#2636=ORIENTED_EDGE('',*,*,#1986,.T.);
#2637=ORIENTED_EDGE('',*,*,#2035,.F.);
#2638=ORIENTED_EDGE('',*,*,#1999,.T.);
#2639=ORIENTED_EDGE('',*,*,#1998,.T.);
#2640=ORIENTED_EDGE('',*,*,#2034,.F.);
#2641=ORIENTED_EDGE('',*,*,#2011,.T.);
#2642=ORIENTED_EDGE('',*,*,#2010,.T.);
#2643=ORIENTED_EDGE('',*,*,#2033,.F.);
#2644=ORIENTED_EDGE('',*,*,#1782,.T.);
#2645=ORIENTED_EDGE('',*,*,#1783,.T.);
#2646=ORIENTED_EDGE('',*,*,#1780,.T.);
#2647=ORIENTED_EDGE('',*,*,#1781,.T.);
#2648=ORIENTED_EDGE('',*,*,#1792,.T.);
#2649=ORIENTED_EDGE('',*,*,#1793,.T.);
#2650=ORIENTED_EDGE('',*,*,#1790,.T.);
#2651=ORIENTED_EDGE('',*,*,#1791,.T.);
#2652=ORIENTED_EDGE('',*,*,#1802,.T.);
#2653=ORIENTED_EDGE('',*,*,#1803,.T.);
#2654=ORIENTED_EDGE('',*,*,#1800,.T.);
#2655=ORIENTED_EDGE('',*,*,#1801,.T.);
#2656=ORIENTED_EDGE('',*,*,#1812,.T.);
#2657=ORIENTED_EDGE('',*,*,#1813,.T.);
#2658=ORIENTED_EDGE('',*,*,#1810,.T.);
#2659=ORIENTED_EDGE('',*,*,#1811,.T.);
#2660=ORIENTED_EDGE('',*,*,#1822,.T.);
#2661=ORIENTED_EDGE('',*,*,#1823,.T.);
#2662=ORIENTED_EDGE('',*,*,#1820,.T.);
#2663=ORIENTED_EDGE('',*,*,#1821,.T.);
#2664=ORIENTED_EDGE('',*,*,#1832,.T.);
#2665=ORIENTED_EDGE('',*,*,#1833,.T.);
#2666=ORIENTED_EDGE('',*,*,#1830,.T.);
#2667=ORIENTED_EDGE('',*,*,#1831,.T.);
#2668=ORIENTED_EDGE('',*,*,#1842,.T.);
#2669=ORIENTED_EDGE('',*,*,#1843,.T.);
#2670=ORIENTED_EDGE('',*,*,#1840,.T.);
#2671=ORIENTED_EDGE('',*,*,#1841,.T.);
#2672=ORIENTED_EDGE('',*,*,#1852,.T.);
#2673=ORIENTED_EDGE('',*,*,#1853,.T.);
#2674=ORIENTED_EDGE('',*,*,#1850,.T.);
#2675=ORIENTED_EDGE('',*,*,#1851,.T.);
#2676=ORIENTED_EDGE('',*,*,#1862,.T.);
#2677=ORIENTED_EDGE('',*,*,#1863,.T.);
#2678=ORIENTED_EDGE('',*,*,#1860,.T.);
#2679=ORIENTED_EDGE('',*,*,#1861,.T.);
#2680=ORIENTED_EDGE('',*,*,#1872,.T.);
#2681=ORIENTED_EDGE('',*,*,#1873,.T.);
#2682=ORIENTED_EDGE('',*,*,#1870,.T.);
#2683=ORIENTED_EDGE('',*,*,#1871,.T.);
#2684=ORIENTED_EDGE('',*,*,#1882,.T.);
#2685=ORIENTED_EDGE('',*,*,#1883,.T.);
#2686=ORIENTED_EDGE('',*,*,#1880,.T.);
#2687=ORIENTED_EDGE('',*,*,#1881,.T.);
#2688=ORIENTED_EDGE('',*,*,#1892,.T.);
#2689=ORIENTED_EDGE('',*,*,#1893,.T.);
#2690=ORIENTED_EDGE('',*,*,#1890,.T.);
#2691=ORIENTED_EDGE('',*,*,#1891,.T.);
#2692=ORIENTED_EDGE('',*,*,#1902,.T.);
#2693=ORIENTED_EDGE('',*,*,#1903,.T.);
#2694=ORIENTED_EDGE('',*,*,#1900,.T.);
#2695=ORIENTED_EDGE('',*,*,#1901,.T.);
#2696=ORIENTED_EDGE('',*,*,#1912,.T.);
#2697=ORIENTED_EDGE('',*,*,#1913,.T.);
#2698=ORIENTED_EDGE('',*,*,#1910,.T.);
#2699=ORIENTED_EDGE('',*,*,#1911,.T.);
#2700=ORIENTED_EDGE('',*,*,#1922,.T.);
#2701=ORIENTED_EDGE('',*,*,#1923,.T.);
#2702=ORIENTED_EDGE('',*,*,#1920,.T.);
#2703=ORIENTED_EDGE('',*,*,#1921,.T.);
#2704=ORIENTED_EDGE('',*,*,#1932,.T.);
#2705=ORIENTED_EDGE('',*,*,#1933,.T.);
#2706=ORIENTED_EDGE('',*,*,#1930,.T.);
#2707=ORIENTED_EDGE('',*,*,#1931,.T.);
#2708=ORIENTED_EDGE('',*,*,#1942,.T.);
#2709=ORIENTED_EDGE('',*,*,#1943,.T.);
#2710=ORIENTED_EDGE('',*,*,#1940,.T.);
#2711=ORIENTED_EDGE('',*,*,#1941,.T.);
#2712=ORIENTED_EDGE('',*,*,#1952,.T.);
#2713=ORIENTED_EDGE('',*,*,#1953,.T.);
#2714=ORIENTED_EDGE('',*,*,#1950,.T.);
#2715=ORIENTED_EDGE('',*,*,#1951,.T.);
#2716=ORIENTED_EDGE('',*,*,#1964,.T.);
#2717=ORIENTED_EDGE('',*,*,#1965,.T.);
#2718=ORIENTED_EDGE('',*,*,#1976,.T.);
#2719=ORIENTED_EDGE('',*,*,#1977,.T.);
#2720=ORIENTED_EDGE('',*,*,#1988,.T.);
#2721=ORIENTED_EDGE('',*,*,#1989,.T.);
#2722=ORIENTED_EDGE('',*,*,#2000,.T.);
#2723=ORIENTED_EDGE('',*,*,#2001,.T.);
#2724=ORIENTED_EDGE('',*,*,#2012,.T.);
#2725=ORIENTED_EDGE('',*,*,#2013,.T.);
#2726=ORIENTED_EDGE('',*,*,#2024,.T.);
#2727=ORIENTED_EDGE('',*,*,#2025,.T.);
#2728=ORIENTED_EDGE('',*,*,#2040,.F.);
#2729=ORIENTED_EDGE('',*,*,#2029,.T.);
#2730=ORIENTED_EDGE('',*,*,#2032,.T.);
#2731=ORIENTED_EDGE('',*,*,#2041,.F.);
#2732=ORIENTED_EDGE('',*,*,#2042,.F.);
#2733=ORIENTED_EDGE('',*,*,#2043,.T.);
#2734=ORIENTED_EDGE('',*,*,#2041,.T.);
#2735=ORIENTED_EDGE('',*,*,#2043,.F.);
#2736=ORIENTED_EDGE('',*,*,#2044,.F.);
#2737=ORIENTED_EDGE('',*,*,#2045,.T.);
#2738=ORIENTED_EDGE('',*,*,#1959,.T.);
#2739=ORIENTED_EDGE('',*,*,#2046,.T.);
#2740=ORIENTED_EDGE('',*,*,#2019,.T.);
#2741=ORIENTED_EDGE('',*,*,#2047,.T.);
#2742=ORIENTED_EDGE('',*,*,#1971,.T.);
#2743=ORIENTED_EDGE('',*,*,#2048,.T.);
#2744=ORIENTED_EDGE('',*,*,#1983,.T.);
#2745=ORIENTED_EDGE('',*,*,#2049,.T.);
#2746=ORIENTED_EDGE('',*,*,#1995,.T.);
#2747=ORIENTED_EDGE('',*,*,#2050,.T.);
#2748=ORIENTED_EDGE('',*,*,#2007,.T.);
#2749=ORIENTED_EDGE('',*,*,#2051,.T.);
#2750=ORIENTED_EDGE('',*,*,#2052,.F.);
#2751=ORIENTED_EDGE('',*,*,#2051,.F.);
#2752=ORIENTED_EDGE('',*,*,#2006,.T.);
#2753=ORIENTED_EDGE('',*,*,#2005,.T.);
#2754=ORIENTED_EDGE('',*,*,#2050,.F.);
#2755=ORIENTED_EDGE('',*,*,#1994,.T.);
#2756=ORIENTED_EDGE('',*,*,#1993,.T.);
#2757=ORIENTED_EDGE('',*,*,#2049,.F.);
#2758=ORIENTED_EDGE('',*,*,#1982,.T.);
#2759=ORIENTED_EDGE('',*,*,#1981,.T.);
#2760=ORIENTED_EDGE('',*,*,#2048,.F.);
#2761=ORIENTED_EDGE('',*,*,#1970,.T.);
#2762=ORIENTED_EDGE('',*,*,#1969,.T.);
#2763=ORIENTED_EDGE('',*,*,#2047,.F.);
#2764=ORIENTED_EDGE('',*,*,#2018,.T.);
#2765=ORIENTED_EDGE('',*,*,#2017,.T.);
#2766=ORIENTED_EDGE('',*,*,#2046,.F.);
#2767=ORIENTED_EDGE('',*,*,#1958,.T.);
#2768=ORIENTED_EDGE('',*,*,#1957,.T.);
#2769=ORIENTED_EDGE('',*,*,#2045,.F.);
#2770=ORIENTED_EDGE('',*,*,#1785,.T.);
#2771=ORIENTED_EDGE('',*,*,#1786,.T.);
#2772=ORIENTED_EDGE('',*,*,#1777,.T.);
#2773=ORIENTED_EDGE('',*,*,#1778,.T.);
#2774=ORIENTED_EDGE('',*,*,#1795,.T.);
#2775=ORIENTED_EDGE('',*,*,#1796,.T.);
#2776=ORIENTED_EDGE('',*,*,#1787,.T.);
#2777=ORIENTED_EDGE('',*,*,#1788,.T.);
#2778=ORIENTED_EDGE('',*,*,#1805,.T.);
#2779=ORIENTED_EDGE('',*,*,#1806,.T.);
#2780=ORIENTED_EDGE('',*,*,#1797,.T.);
#2781=ORIENTED_EDGE('',*,*,#1798,.T.);
#2782=ORIENTED_EDGE('',*,*,#1815,.T.);
#2783=ORIENTED_EDGE('',*,*,#1816,.T.);
#2784=ORIENTED_EDGE('',*,*,#1807,.T.);
#2785=ORIENTED_EDGE('',*,*,#1808,.T.);
#2786=ORIENTED_EDGE('',*,*,#1825,.T.);
#2787=ORIENTED_EDGE('',*,*,#1826,.T.);
#2788=ORIENTED_EDGE('',*,*,#1817,.T.);
#2789=ORIENTED_EDGE('',*,*,#1818,.T.);
#2790=ORIENTED_EDGE('',*,*,#1835,.T.);
#2791=ORIENTED_EDGE('',*,*,#1836,.T.);
#2792=ORIENTED_EDGE('',*,*,#1827,.T.);
#2793=ORIENTED_EDGE('',*,*,#1828,.T.);
#2794=ORIENTED_EDGE('',*,*,#1845,.T.);
#2795=ORIENTED_EDGE('',*,*,#1846,.T.);
#2796=ORIENTED_EDGE('',*,*,#1837,.T.);
#2797=ORIENTED_EDGE('',*,*,#1838,.T.);
#2798=ORIENTED_EDGE('',*,*,#1855,.T.);
#2799=ORIENTED_EDGE('',*,*,#1856,.T.);
#2800=ORIENTED_EDGE('',*,*,#1847,.T.);
#2801=ORIENTED_EDGE('',*,*,#1848,.T.);
#2802=ORIENTED_EDGE('',*,*,#1865,.T.);
#2803=ORIENTED_EDGE('',*,*,#1866,.T.);
#2804=ORIENTED_EDGE('',*,*,#1857,.T.);
#2805=ORIENTED_EDGE('',*,*,#1858,.T.);
#2806=ORIENTED_EDGE('',*,*,#1875,.T.);
#2807=ORIENTED_EDGE('',*,*,#1876,.T.);
#2808=ORIENTED_EDGE('',*,*,#1867,.T.);
#2809=ORIENTED_EDGE('',*,*,#1868,.T.);
#2810=ORIENTED_EDGE('',*,*,#1885,.T.);
#2811=ORIENTED_EDGE('',*,*,#1886,.T.);
#2812=ORIENTED_EDGE('',*,*,#1877,.T.);
#2813=ORIENTED_EDGE('',*,*,#1878,.T.);
#2814=ORIENTED_EDGE('',*,*,#1895,.T.);
#2815=ORIENTED_EDGE('',*,*,#1896,.T.);
#2816=ORIENTED_EDGE('',*,*,#1887,.T.);
#2817=ORIENTED_EDGE('',*,*,#1888,.T.);
#2818=ORIENTED_EDGE('',*,*,#1905,.T.);
#2819=ORIENTED_EDGE('',*,*,#1906,.T.);
#2820=ORIENTED_EDGE('',*,*,#1897,.T.);
#2821=ORIENTED_EDGE('',*,*,#1898,.T.);
#2822=ORIENTED_EDGE('',*,*,#1915,.T.);
#2823=ORIENTED_EDGE('',*,*,#1916,.T.);
#2824=ORIENTED_EDGE('',*,*,#1907,.T.);
#2825=ORIENTED_EDGE('',*,*,#1908,.T.);
#2826=ORIENTED_EDGE('',*,*,#1925,.T.);
#2827=ORIENTED_EDGE('',*,*,#1926,.T.);
#2828=ORIENTED_EDGE('',*,*,#1917,.T.);
#2829=ORIENTED_EDGE('',*,*,#1918,.T.);
#2830=ORIENTED_EDGE('',*,*,#1935,.T.);
#2831=ORIENTED_EDGE('',*,*,#1936,.T.);
#2832=ORIENTED_EDGE('',*,*,#1927,.T.);
#2833=ORIENTED_EDGE('',*,*,#1928,.T.);
#2834=ORIENTED_EDGE('',*,*,#1945,.T.);
#2835=ORIENTED_EDGE('',*,*,#1946,.T.);
#2836=ORIENTED_EDGE('',*,*,#1937,.T.);
#2837=ORIENTED_EDGE('',*,*,#1938,.T.);
#2838=ORIENTED_EDGE('',*,*,#1955,.T.);
#2839=ORIENTED_EDGE('',*,*,#1956,.T.);
#2840=ORIENTED_EDGE('',*,*,#1947,.T.);
#2841=ORIENTED_EDGE('',*,*,#1948,.T.);
#2842=ORIENTED_EDGE('',*,*,#1967,.T.);
#2843=ORIENTED_EDGE('',*,*,#1968,.T.);
#2844=ORIENTED_EDGE('',*,*,#1979,.T.);
#2845=ORIENTED_EDGE('',*,*,#1980,.T.);
#2846=ORIENTED_EDGE('',*,*,#1991,.T.);
#2847=ORIENTED_EDGE('',*,*,#1992,.T.);
#2848=ORIENTED_EDGE('',*,*,#2003,.T.);
#2849=ORIENTED_EDGE('',*,*,#2004,.T.);
#2850=ORIENTED_EDGE('',*,*,#2015,.T.);
#2851=ORIENTED_EDGE('',*,*,#2016,.T.);
#2852=ORIENTED_EDGE('',*,*,#2027,.T.);
#2853=ORIENTED_EDGE('',*,*,#2028,.T.);
#2854=ORIENTED_EDGE('',*,*,#2044,.T.);
#2855=ORIENTED_EDGE('',*,*,#2031,.T.);
#2856=ORIENTED_EDGE('',*,*,#2053,.F.);
#2857=ORIENTED_EDGE('',*,*,#2054,.F.);
#2858=ORIENTED_EDGE('',*,*,#2055,.F.);
#2859=ORIENTED_EDGE('',*,*,#2056,.T.);
#2860=ORIENTED_EDGE('',*,*,#2053,.T.);
#2861=ORIENTED_EDGE('',*,*,#2056,.F.);
#2862=ORIENTED_EDGE('',*,*,#2054,.T.);
#2863=ORIENTED_EDGE('',*,*,#2057,.T.);
#2864=ORIENTED_EDGE('',*,*,#2058,.T.);
#2865=ORIENTED_EDGE('',*,*,#2057,.F.);
#2866=ORIENTED_EDGE('',*,*,#2055,.T.);
#2867=ORIENTED_EDGE('',*,*,#2052,.T.);
#2868=ORIENTED_EDGE('',*,*,#2058,.F.);
#2869=ORIENTED_EDGE('',*,*,#2042,.T.);
#2870=ORIENTED_EDGE('',*,*,#2059,.F.);
#2871=ORIENTED_EDGE('',*,*,#2060,.T.);
#2872=ORIENTED_EDGE('',*,*,#2061,.T.);
#2873=ORIENTED_EDGE('',*,*,#2060,.F.);
#2874=ORIENTED_EDGE('',*,*,#2062,.F.);
#2875=ORIENTED_EDGE('',*,*,#2063,.T.);
#2876=ORIENTED_EDGE('',*,*,#2064,.T.);
#2877=ORIENTED_EDGE('',*,*,#2063,.F.);
#2878=ORIENTED_EDGE('',*,*,#2062,.T.);
#2879=ORIENTED_EDGE('',*,*,#2059,.T.);
#2880=ORIENTED_EDGE('',*,*,#2064,.F.);
#2881=ORIENTED_EDGE('',*,*,#2061,.F.);
#2882=ORIENTED_EDGE('',*,*,#2065,.F.);
#2883=ORIENTED_EDGE('',*,*,#2066,.T.);
#2884=ORIENTED_EDGE('',*,*,#2067,.T.);
#2885=ORIENTED_EDGE('',*,*,#2066,.F.);
#2886=ORIENTED_EDGE('',*,*,#2068,.F.);
#2887=ORIENTED_EDGE('',*,*,#2069,.T.);
#2888=ORIENTED_EDGE('',*,*,#2070,.T.);
#2889=ORIENTED_EDGE('',*,*,#2069,.F.);
#2890=ORIENTED_EDGE('',*,*,#2068,.T.);
#2891=ORIENTED_EDGE('',*,*,#2065,.T.);
#2892=ORIENTED_EDGE('',*,*,#2070,.F.);
#2893=ORIENTED_EDGE('',*,*,#2067,.F.);
#2894=ORIENTED_EDGE('',*,*,#2071,.F.);
#2895=ORIENTED_EDGE('',*,*,#2072,.T.);
#2896=ORIENTED_EDGE('',*,*,#2073,.F.);
#2897=ORIENTED_EDGE('',*,*,#2072,.F.);
#2898=ORIENTED_EDGE('',*,*,#2074,.F.);
#2899=ORIENTED_EDGE('',*,*,#2075,.T.);
#2900=ORIENTED_EDGE('',*,*,#2076,.F.);
#2901=ORIENTED_EDGE('',*,*,#2075,.F.);
#2902=ORIENTED_EDGE('',*,*,#2077,.F.);
#2903=ORIENTED_EDGE('',*,*,#2078,.T.);
#2904=ORIENTED_EDGE('',*,*,#2079,.F.);
#2905=ORIENTED_EDGE('',*,*,#2078,.F.);
#2906=ORIENTED_EDGE('',*,*,#2080,.F.);
#2907=ORIENTED_EDGE('',*,*,#2081,.T.);
#2908=ORIENTED_EDGE('',*,*,#2082,.F.);
#2909=ORIENTED_EDGE('',*,*,#2081,.F.);
#2910=ORIENTED_EDGE('',*,*,#2083,.F.);
#2911=ORIENTED_EDGE('',*,*,#2084,.T.);
#2912=ORIENTED_EDGE('',*,*,#2085,.T.);
#2913=ORIENTED_EDGE('',*,*,#2084,.F.);
#2914=ORIENTED_EDGE('',*,*,#2086,.F.);
#2915=ORIENTED_EDGE('',*,*,#2087,.T.);
#2916=ORIENTED_EDGE('',*,*,#2088,.T.);
#2917=ORIENTED_EDGE('',*,*,#2087,.F.);
#2918=ORIENTED_EDGE('',*,*,#2086,.T.);
#2919=ORIENTED_EDGE('',*,*,#2083,.T.);
#2920=ORIENTED_EDGE('',*,*,#2082,.T.);
#2921=ORIENTED_EDGE('',*,*,#2079,.T.);
#2922=ORIENTED_EDGE('',*,*,#2076,.T.);
#2923=ORIENTED_EDGE('',*,*,#2073,.T.);
#2924=ORIENTED_EDGE('',*,*,#2088,.F.);
#2925=ORIENTED_EDGE('',*,*,#2085,.F.);
#2926=ORIENTED_EDGE('',*,*,#2080,.T.);
#2927=ORIENTED_EDGE('',*,*,#2077,.T.);
#2928=ORIENTED_EDGE('',*,*,#2074,.T.);
#2929=ORIENTED_EDGE('',*,*,#2071,.T.);
#2930=ORIENTED_EDGE('',*,*,#2089,.F.);
#2931=ORIENTED_EDGE('',*,*,#2090,.T.);
#2932=ORIENTED_EDGE('',*,*,#2091,.F.);
#2933=ORIENTED_EDGE('',*,*,#2090,.F.);
#2934=ORIENTED_EDGE('',*,*,#2092,.F.);
#2935=ORIENTED_EDGE('',*,*,#2093,.T.);
#2936=ORIENTED_EDGE('',*,*,#2094,.F.);
#2937=ORIENTED_EDGE('',*,*,#2093,.F.);
#2938=ORIENTED_EDGE('',*,*,#2095,.F.);
#2939=ORIENTED_EDGE('',*,*,#2096,.T.);
#2940=ORIENTED_EDGE('',*,*,#2097,.F.);
#2941=ORIENTED_EDGE('',*,*,#2096,.F.);
#2942=ORIENTED_EDGE('',*,*,#2098,.F.);
#2943=ORIENTED_EDGE('',*,*,#2099,.T.);
#2944=ORIENTED_EDGE('',*,*,#2100,.F.);
#2945=ORIENTED_EDGE('',*,*,#2099,.F.);
#2946=ORIENTED_EDGE('',*,*,#2101,.F.);
#2947=ORIENTED_EDGE('',*,*,#2102,.T.);
#2948=ORIENTED_EDGE('',*,*,#2103,.F.);
#2949=ORIENTED_EDGE('',*,*,#2102,.F.);
#2950=ORIENTED_EDGE('',*,*,#2104,.F.);
#2951=ORIENTED_EDGE('',*,*,#2105,.T.);
#2952=ORIENTED_EDGE('',*,*,#2106,.T.);
#2953=ORIENTED_EDGE('',*,*,#2105,.F.);
#2954=ORIENTED_EDGE('',*,*,#2106,.F.);
#2955=ORIENTED_EDGE('',*,*,#2101,.T.);
#2956=ORIENTED_EDGE('',*,*,#2107,.F.);
#2957=ORIENTED_EDGE('',*,*,#2108,.T.);
#2958=ORIENTED_EDGE('',*,*,#2109,.T.);
#2959=ORIENTED_EDGE('',*,*,#2108,.F.);
#2960=ORIENTED_EDGE('',*,*,#2107,.T.);
#2961=ORIENTED_EDGE('',*,*,#2103,.T.);
#2962=ORIENTED_EDGE('',*,*,#2100,.T.);
#2963=ORIENTED_EDGE('',*,*,#2097,.T.);
#2964=ORIENTED_EDGE('',*,*,#2094,.T.);
#2965=ORIENTED_EDGE('',*,*,#2091,.T.);
#2966=ORIENTED_EDGE('',*,*,#2109,.F.);
#2967=ORIENTED_EDGE('',*,*,#2104,.T.);
#2968=ORIENTED_EDGE('',*,*,#2098,.T.);
#2969=ORIENTED_EDGE('',*,*,#2095,.T.);
#2970=ORIENTED_EDGE('',*,*,#2092,.T.);
#2971=ORIENTED_EDGE('',*,*,#2089,.T.);
#2972=ORIENTED_EDGE('',*,*,#2110,.F.);
#2973=ORIENTED_EDGE('',*,*,#2111,.F.);
#2974=ORIENTED_EDGE('',*,*,#2112,.T.);
#2975=ORIENTED_EDGE('',*,*,#2110,.T.);
#2976=ORIENTED_EDGE('',*,*,#2112,.F.);
#2977=ORIENTED_EDGE('',*,*,#2113,.F.);
#2978=ORIENTED_EDGE('',*,*,#2114,.T.);
#2979=ORIENTED_EDGE('',*,*,#2111,.T.);
#2980=ORIENTED_EDGE('',*,*,#2114,.F.);
#2981=ORIENTED_EDGE('',*,*,#2115,.F.);
#2982=ORIENTED_EDGE('',*,*,#2116,.T.);
#2983=ORIENTED_EDGE('',*,*,#2113,.T.);
#2984=ORIENTED_EDGE('',*,*,#2116,.F.);
#2985=ORIENTED_EDGE('',*,*,#2115,.T.);
#2986=ORIENTED_EDGE('',*,*,#2117,.F.);
#2987=ORIENTED_EDGE('',*,*,#2118,.F.);
#2988=ORIENTED_EDGE('',*,*,#2119,.T.);
#2989=ORIENTED_EDGE('',*,*,#2117,.T.);
#2990=ORIENTED_EDGE('',*,*,#2119,.F.);
#2991=ORIENTED_EDGE('',*,*,#2120,.F.);
#2992=ORIENTED_EDGE('',*,*,#2121,.T.);
#2993=ORIENTED_EDGE('',*,*,#2118,.T.);
#2994=ORIENTED_EDGE('',*,*,#2121,.F.);
#2995=ORIENTED_EDGE('',*,*,#2122,.F.);
#2996=ORIENTED_EDGE('',*,*,#2123,.T.);
#2997=ORIENTED_EDGE('',*,*,#2120,.T.);
#2998=ORIENTED_EDGE('',*,*,#2123,.F.);
#2999=ORIENTED_EDGE('',*,*,#2122,.T.);
#3000=ORIENTED_EDGE('',*,*,#2124,.T.);
#3001=ORIENTED_EDGE('',*,*,#2125,.T.);
#3002=ORIENTED_EDGE('',*,*,#2126,.T.);
#3003=ORIENTED_EDGE('',*,*,#2127,.F.);
#3004=ORIENTED_EDGE('',*,*,#2128,.T.);
#3005=ORIENTED_EDGE('',*,*,#2129,.T.);
#3006=ORIENTED_EDGE('',*,*,#2130,.T.);
#3007=ORIENTED_EDGE('',*,*,#2125,.F.);
#3008=ORIENTED_EDGE('',*,*,#2131,.T.);
#3009=ORIENTED_EDGE('',*,*,#2132,.T.);
#3010=ORIENTED_EDGE('',*,*,#2133,.T.);
#3011=ORIENTED_EDGE('',*,*,#2129,.F.);
#3012=ORIENTED_EDGE('',*,*,#2134,.T.);
#3013=ORIENTED_EDGE('',*,*,#2135,.T.);
#3014=ORIENTED_EDGE('',*,*,#2136,.T.);
#3015=ORIENTED_EDGE('',*,*,#2132,.F.);
#3016=ORIENTED_EDGE('',*,*,#2137,.T.);
#3017=ORIENTED_EDGE('',*,*,#2138,.T.);
#3018=ORIENTED_EDGE('',*,*,#2139,.T.);
#3019=ORIENTED_EDGE('',*,*,#2135,.F.);
#3020=ORIENTED_EDGE('',*,*,#2140,.T.);
#3021=ORIENTED_EDGE('',*,*,#2127,.T.);
#3022=ORIENTED_EDGE('',*,*,#2141,.T.);
#3023=ORIENTED_EDGE('',*,*,#2138,.F.);
#3024=ORIENTED_EDGE('',*,*,#2140,.F.);
#3025=ORIENTED_EDGE('',*,*,#2137,.F.);
#3026=ORIENTED_EDGE('',*,*,#2134,.F.);
#3027=ORIENTED_EDGE('',*,*,#2131,.F.);
#3028=ORIENTED_EDGE('',*,*,#2128,.F.);
#3029=ORIENTED_EDGE('',*,*,#2124,.F.);
#3030=ORIENTED_EDGE('',*,*,#2141,.F.);
#3031=ORIENTED_EDGE('',*,*,#2126,.F.);
#3032=ORIENTED_EDGE('',*,*,#2130,.F.);
#3033=ORIENTED_EDGE('',*,*,#2133,.F.);
#3034=ORIENTED_EDGE('',*,*,#2136,.F.);
#3035=ORIENTED_EDGE('',*,*,#2139,.F.);
#3036=ORIENTED_EDGE('',*,*,#2142,.T.);
#3037=ORIENTED_EDGE('',*,*,#2143,.T.);
#3038=ORIENTED_EDGE('',*,*,#2144,.T.);
#3039=ORIENTED_EDGE('',*,*,#2145,.T.);
#3040=ORIENTED_EDGE('',*,*,#2146,.T.);
#3041=ORIENTED_EDGE('',*,*,#2147,.T.);
#3042=ORIENTED_EDGE('',*,*,#2148,.F.);
#3043=ORIENTED_EDGE('',*,*,#2149,.T.);
#3044=ORIENTED_EDGE('',*,*,#2150,.T.);
#3045=ORIENTED_EDGE('',*,*,#2151,.T.);
#3046=ORIENTED_EDGE('',*,*,#2152,.T.);
#3047=ORIENTED_EDGE('',*,*,#2153,.T.);
#3048=ORIENTED_EDGE('',*,*,#2154,.T.);
#3049=ORIENTED_EDGE('',*,*,#2155,.F.);
#3050=ORIENTED_EDGE('',*,*,#2156,.F.);
#3051=ORIENTED_EDGE('',*,*,#2154,.F.);
#3052=ORIENTED_EDGE('',*,*,#2157,.F.);
#3053=ORIENTED_EDGE('',*,*,#2143,.F.);
#3054=ORIENTED_EDGE('',*,*,#2157,.T.);
#3055=ORIENTED_EDGE('',*,*,#2153,.F.);
#3056=ORIENTED_EDGE('',*,*,#2158,.F.);
#3057=ORIENTED_EDGE('',*,*,#2144,.F.);
#3058=ORIENTED_EDGE('',*,*,#2158,.T.);
#3059=ORIENTED_EDGE('',*,*,#2152,.F.);
#3060=ORIENTED_EDGE('',*,*,#2159,.F.);
#3061=ORIENTED_EDGE('',*,*,#2145,.F.);
#3062=ORIENTED_EDGE('',*,*,#2159,.T.);
#3063=ORIENTED_EDGE('',*,*,#2151,.F.);
#3064=ORIENTED_EDGE('',*,*,#2160,.F.);
#3065=ORIENTED_EDGE('',*,*,#2146,.F.);
#3066=ORIENTED_EDGE('',*,*,#2160,.T.);
#3067=ORIENTED_EDGE('',*,*,#2150,.F.);
#3068=ORIENTED_EDGE('',*,*,#2161,.F.);
#3069=ORIENTED_EDGE('',*,*,#2147,.F.);
#3070=ORIENTED_EDGE('',*,*,#2161,.T.);
#3071=ORIENTED_EDGE('',*,*,#2149,.F.);
#3072=ORIENTED_EDGE('',*,*,#2156,.T.);
#3073=ORIENTED_EDGE('',*,*,#2142,.F.);
#3074=ORIENTED_EDGE('',*,*,#2155,.T.);
#3075=ORIENTED_EDGE('',*,*,#2162,.T.);
#3076=ORIENTED_EDGE('',*,*,#2163,.T.);
#3077=ORIENTED_EDGE('',*,*,#2162,.F.);
#3078=ORIENTED_EDGE('',*,*,#2164,.F.);
#3079=ORIENTED_EDGE('',*,*,#2165,.T.);
#3080=ORIENTED_EDGE('',*,*,#2163,.F.);
#3081=ORIENTED_EDGE('',*,*,#2166,.T.);
#3082=ORIENTED_EDGE('',*,*,#2164,.T.);
#3083=ORIENTED_EDGE('',*,*,#2166,.F.);
#3084=ORIENTED_EDGE('',*,*,#2167,.F.);
#3085=ORIENTED_EDGE('',*,*,#2168,.T.);
#3086=ORIENTED_EDGE('',*,*,#2148,.T.);
#3087=ORIENTED_EDGE('',*,*,#2168,.F.);
#3088=ORIENTED_EDGE('',*,*,#2169,.F.);
#3089=ORIENTED_EDGE('',*,*,#2170,.T.);
#3090=ORIENTED_EDGE('',*,*,#2167,.T.);
#3091=ORIENTED_EDGE('',*,*,#2170,.F.);
#3092=ORIENTED_EDGE('',*,*,#2169,.T.);
#3093=ORIENTED_EDGE('',*,*,#2171,.F.);
#3094=ORIENTED_EDGE('',*,*,#2171,.T.);
#3095=ORIENTED_EDGE('',*,*,#2172,.T.);
#3096=ORIENTED_EDGE('',*,*,#2165,.F.);
#3097=ORIENTED_EDGE('',*,*,#2172,.F.);
#3098=ORIENTED_EDGE('',*,*,#2173,.F.);
#3099=ORIENTED_EDGE('',*,*,#2174,.F.);
#3100=ORIENTED_EDGE('',*,*,#2175,.F.);
#3101=ORIENTED_EDGE('',*,*,#2176,.F.);
#3102=ORIENTED_EDGE('',*,*,#2177,.F.);
#3103=ORIENTED_EDGE('',*,*,#2178,.F.);
#3104=ORIENTED_EDGE('',*,*,#2179,.T.);
#3105=ORIENTED_EDGE('',*,*,#2174,.T.);
#3106=ORIENTED_EDGE('',*,*,#2180,.T.);
#3107=ORIENTED_EDGE('',*,*,#2181,.F.);
#3108=ORIENTED_EDGE('',*,*,#2182,.F.);
#3109=ORIENTED_EDGE('',*,*,#2175,.T.);
#3110=ORIENTED_EDGE('',*,*,#2182,.T.);
#3111=ORIENTED_EDGE('',*,*,#2183,.F.);
#3112=ORIENTED_EDGE('',*,*,#2184,.F.);
#3113=ORIENTED_EDGE('',*,*,#2176,.T.);
#3114=ORIENTED_EDGE('',*,*,#2184,.T.);
#3115=ORIENTED_EDGE('',*,*,#2185,.F.);
#3116=ORIENTED_EDGE('',*,*,#2186,.F.);
#3117=ORIENTED_EDGE('',*,*,#2177,.T.);
#3118=ORIENTED_EDGE('',*,*,#2186,.T.);
#3119=ORIENTED_EDGE('',*,*,#2187,.F.);
#3120=ORIENTED_EDGE('',*,*,#2188,.F.);
#3121=ORIENTED_EDGE('',*,*,#2178,.T.);
#3122=ORIENTED_EDGE('',*,*,#2188,.T.);
#3123=ORIENTED_EDGE('',*,*,#2189,.F.);
#3124=ORIENTED_EDGE('',*,*,#2190,.F.);
#3125=ORIENTED_EDGE('',*,*,#2173,.T.);
#3126=ORIENTED_EDGE('',*,*,#2190,.T.);
#3127=ORIENTED_EDGE('',*,*,#2191,.F.);
#3128=ORIENTED_EDGE('',*,*,#2180,.F.);
#3129=ORIENTED_EDGE('',*,*,#2191,.T.);
#3130=ORIENTED_EDGE('',*,*,#2189,.T.);
#3131=ORIENTED_EDGE('',*,*,#2187,.T.);
#3132=ORIENTED_EDGE('',*,*,#2185,.T.);
#3133=ORIENTED_EDGE('',*,*,#2183,.T.);
#3134=ORIENTED_EDGE('',*,*,#2181,.T.);
#3135=ORIENTED_EDGE('',*,*,#2179,.F.);
#3136=ORIENTED_EDGE('',*,*,#2192,.T.);
#3137=ORIENTED_EDGE('',*,*,#2193,.T.);
#3138=ORIENTED_EDGE('',*,*,#2192,.F.);
#3139=ORIENTED_EDGE('',*,*,#2193,.F.);
#3140=CYLINDRICAL_SURFACE('',#3496,0.25);
#3141=CYLINDRICAL_SURFACE('',#3499,0.25);
#3142=CYLINDRICAL_SURFACE('',#3502,0.25);
#3143=CYLINDRICAL_SURFACE('',#3505,0.25);
#3144=CYLINDRICAL_SURFACE('',#3513,1.6);
#3145=CYLINDRICAL_SURFACE('',#3518,1.01);
#3146=CYLINDRICAL_SURFACE('',#3525,0.79);
#3147=CYLINDRICAL_SURFACE('',#3531,0.8);
#3148=CYLINDRICAL_SURFACE('',#3532,0.93);
#3149=CYLINDRICAL_SURFACE('',#3537,0.93);
#3150=CYLINDRICAL_SURFACE('',#3541,0.79);
#3151=CYLINDRICAL_SURFACE('',#3545,3.);
#3152=CYLINDRICAL_SURFACE('',#3547,2.);
#3153=CYLINDRICAL_SURFACE('',#3552,2.);
#3154=CYLINDRICAL_SURFACE('',#3558,0.0999999999999996);
#3155=CYLINDRICAL_SURFACE('',#3559,0.0999999999999996);
#3156=CYLINDRICAL_SURFACE('',#3560,0.0999999999999996);
#3157=CYLINDRICAL_SURFACE('',#3561,0.0999999999999996);
#3158=CYLINDRICAL_SURFACE('',#3562,0.1);
#3159=CYLINDRICAL_SURFACE('',#3563,0.1);
#3160=CYLINDRICAL_SURFACE('',#3564,0.1);
#3161=CYLINDRICAL_SURFACE('',#3565,0.1);
#3162=CYLINDRICAL_SURFACE('',#3566,0.1);
#3163=CYLINDRICAL_SURFACE('',#3567,0.1);
#3164=CYLINDRICAL_SURFACE('',#3568,0.0999999999999996);
#3165=CYLINDRICAL_SURFACE('',#3569,0.0999999999999996);
#3166=CYLINDRICAL_SURFACE('',#3570,0.0999999999999996);
#3167=CYLINDRICAL_SURFACE('',#3571,0.0999999999999996);
#3168=CYLINDRICAL_SURFACE('',#3572,0.0999999999999996);
#3169=CYLINDRICAL_SURFACE('',#3573,0.0999999999999996);
#3170=CYLINDRICAL_SURFACE('',#3574,0.1);
#3171=CYLINDRICAL_SURFACE('',#3575,0.1);
#3172=CYLINDRICAL_SURFACE('',#3576,0.1);
#3173=CYLINDRICAL_SURFACE('',#3577,0.1);
#3174=CYLINDRICAL_SURFACE('',#3578,0.1);
#3175=CYLINDRICAL_SURFACE('',#3579,0.1);
#3176=CYLINDRICAL_SURFACE('',#3580,0.0999999999999996);
#3177=CYLINDRICAL_SURFACE('',#3581,0.0999999999999996);
#3178=CYLINDRICAL_SURFACE('',#3582,0.0999999999999996);
#3179=CYLINDRICAL_SURFACE('',#3583,0.0999999999999996);
#3180=CYLINDRICAL_SURFACE('',#3584,0.0999999999999996);
#3181=CYLINDRICAL_SURFACE('',#3585,0.0999999999999996);
#3182=CYLINDRICAL_SURFACE('',#3586,0.1);
#3183=CYLINDRICAL_SURFACE('',#3587,0.1);
#3184=CYLINDRICAL_SURFACE('',#3588,0.1);
#3185=CYLINDRICAL_SURFACE('',#3589,0.1);
#3186=CYLINDRICAL_SURFACE('',#3590,0.1);
#3187=CYLINDRICAL_SURFACE('',#3591,0.1);
#3188=CYLINDRICAL_SURFACE('',#3592,0.0999999999999996);
#3189=CYLINDRICAL_SURFACE('',#3593,0.0999999999999996);
#3190=CYLINDRICAL_SURFACE('',#3594,0.0999999999999996);
#3191=CYLINDRICAL_SURFACE('',#3595,0.0999999999999996);
#3192=CYLINDRICAL_SURFACE('',#3596,0.0999999999999996);
#3193=CYLINDRICAL_SURFACE('',#3597,0.0999999999999996);
#3194=CYLINDRICAL_SURFACE('',#3598,0.1);
#3195=CYLINDRICAL_SURFACE('',#3599,0.1);
#3196=CYLINDRICAL_SURFACE('',#3600,0.1);
#3197=CYLINDRICAL_SURFACE('',#3601,0.1);
#3198=CYLINDRICAL_SURFACE('',#3602,0.1);
#3199=CYLINDRICAL_SURFACE('',#3603,0.1);
#3200=CYLINDRICAL_SURFACE('',#3604,0.0999999999999996);
#3201=CYLINDRICAL_SURFACE('',#3605,0.0999999999999996);
#3202=CYLINDRICAL_SURFACE('',#3606,0.685);
#3203=CYLINDRICAL_SURFACE('',#3609,1.);
#3204=CYLINDRICAL_SURFACE('',#3615,0.8);
#3205=CYLINDRICAL_SURFACE('',#3617,1.1);
#3206=CYLINDRICAL_SURFACE('',#3624,1.4);
#3207=CYLINDRICAL_SURFACE('',#3626,1.);
#3208=CYLINDRICAL_SURFACE('',#3631,1.01);
#3209=CYLINDRICAL_SURFACE('',#3634,1.4);
#3210=CYLINDRICAL_SURFACE('',#3640,0.685);
#3211=CYLINDRICAL_SURFACE('',#3643,1.1);
#3212=CYLINDRICAL_SURFACE('',#3649,0.33);
#3213=CYLINDRICAL_SURFACE('',#3652,0.33);
#3214=CYLINDRICAL_SURFACE('',#3655,0.33);
#3215=CYLINDRICAL_SURFACE('',#3658,0.33);
#3216=CYLINDRICAL_SURFACE('',#3661,1.6);
#3217=CYLINDRICAL_SURFACE('',#3664,3.);
#3218=CYLINDRICAL_SURFACE('',#3670,0.33);
#3219=CYLINDRICAL_SURFACE('',#3673,0.33);
#3220=CYLINDRICAL_SURFACE('',#3676,0.33);
#3221=CYLINDRICAL_SURFACE('',#3679,0.33);
#3222=CYLINDRICAL_SURFACE('',#3682,0.685);
#3223=CYLINDRICAL_SURFACE('',#3685,1.3);
#3224=CYLINDRICAL_SURFACE('',#3689,3.);
#3225=CYLINDRICAL_SURFACE('',#3699,0.5);
#3226=CYLINDRICAL_SURFACE('',#3707,0.2942);
#3227=CYLINDRICAL_SURFACE('',#3731,1.065);
#3228=CYLINDRICAL_SURFACE('',#3737,1.065);
#3229=CYLINDRICAL_SURFACE('',#3743,0.79);
#3230=CYLINDRICAL_SURFACE('',#3754,0.685);
#3231=ADVANCED_FACE('',(#520),#3140,.F.);
#3232=ADVANCED_FACE('',(#521),#3141,.F.);
#3233=ADVANCED_FACE('',(#522),#3142,.F.);
#3234=ADVANCED_FACE('',(#523),#3143,.F.);
#3235=ADVANCED_FACE('',(#524,#319),#465,.T.);
#3236=ADVANCED_FACE('',(#525),#3144,.F.);
#3237=ADVANCED_FACE('',(#526),#466,.T.);
#3238=ADVANCED_FACE('',(#527),#3145,.F.);
#3239=ADVANCED_FACE('',(#528),#467,.T.);
#3240=ADVANCED_FACE('',(#529),#3146,.F.);
#3241=ADVANCED_FACE('',(#530),#468,.T.);
#3242=ADVANCED_FACE('',(#531),#3147,.F.);
#3243=ADVANCED_FACE('',(#532),#3148,.F.);
#3244=ADVANCED_FACE('',(#533,#320),#469,.T.);
#3245=ADVANCED_FACE('',(#534),#3149,.F.);
#3246=ADVANCED_FACE('',(#535,#321),#470,.F.);
#3247=ADVANCED_FACE('',(#536),#3150,.F.);
#3248=ADVANCED_FACE('',(#537,#322,#323,#324,#325,#326),#471,.F.);
#3249=ADVANCED_FACE('',(#538),#3151,.T.);
#3250=ADVANCED_FACE('',(#539),#3152,.T.);
#3251=ADVANCED_FACE('',(#540,#327,#328,#329,#330,#331),#472,.T.);
#3252=ADVANCED_FACE('',(#541,#332),#3153,.T.);
#3253=ADVANCED_FACE('',(#542,#333),#473,.T.);
#3254=ADVANCED_FACE('',(#543,#334),#474,.F.);
#3255=ADVANCED_FACE('',(#544),#3154,.F.);
#3256=ADVANCED_FACE('',(#545),#3155,.F.);
#3257=ADVANCED_FACE('',(#546),#3156,.F.);
#3258=ADVANCED_FACE('',(#547),#3157,.F.);
#3259=ADVANCED_FACE('',(#548),#3158,.F.);
#3260=ADVANCED_FACE('',(#549),#3159,.F.);
#3261=ADVANCED_FACE('',(#550),#3160,.F.);
#3262=ADVANCED_FACE('',(#551),#3161,.F.);
#3263=ADVANCED_FACE('',(#552),#3162,.F.);
#3264=ADVANCED_FACE('',(#553),#3163,.F.);
#3265=ADVANCED_FACE('',(#554),#3164,.F.);
#3266=ADVANCED_FACE('',(#555),#3165,.F.);
#3267=ADVANCED_FACE('',(#556),#3166,.F.);
#3268=ADVANCED_FACE('',(#557),#3167,.F.);
#3269=ADVANCED_FACE('',(#558),#3168,.F.);
#3270=ADVANCED_FACE('',(#559),#3169,.F.);
#3271=ADVANCED_FACE('',(#560),#3170,.F.);
#3272=ADVANCED_FACE('',(#561),#3171,.F.);
#3273=ADVANCED_FACE('',(#562),#3172,.F.);
#3274=ADVANCED_FACE('',(#563),#3173,.F.);
#3275=ADVANCED_FACE('',(#564),#3174,.F.);
#3276=ADVANCED_FACE('',(#565),#3175,.F.);
#3277=ADVANCED_FACE('',(#566),#3176,.F.);
#3278=ADVANCED_FACE('',(#567),#3177,.F.);
#3279=ADVANCED_FACE('',(#568),#3178,.F.);
#3280=ADVANCED_FACE('',(#569),#3179,.F.);
#3281=ADVANCED_FACE('',(#570),#3180,.F.);
#3282=ADVANCED_FACE('',(#571),#3181,.F.);
#3283=ADVANCED_FACE('',(#572),#3182,.F.);
#3284=ADVANCED_FACE('',(#573),#3183,.F.);
#3285=ADVANCED_FACE('',(#574),#3184,.F.);
#3286=ADVANCED_FACE('',(#575),#3185,.F.);
#3287=ADVANCED_FACE('',(#576),#3186,.F.);
#3288=ADVANCED_FACE('',(#577),#3187,.F.);
#3289=ADVANCED_FACE('',(#578),#3188,.F.);
#3290=ADVANCED_FACE('',(#579),#3189,.F.);
#3291=ADVANCED_FACE('',(#580),#3190,.F.);
#3292=ADVANCED_FACE('',(#581),#3191,.F.);
#3293=ADVANCED_FACE('',(#582),#3192,.F.);
#3294=ADVANCED_FACE('',(#583),#3193,.F.);
#3295=ADVANCED_FACE('',(#584),#3194,.F.);
#3296=ADVANCED_FACE('',(#585),#3195,.F.);
#3297=ADVANCED_FACE('',(#586),#3196,.F.);
#3298=ADVANCED_FACE('',(#587),#3197,.F.);
#3299=ADVANCED_FACE('',(#588),#3198,.F.);
#3300=ADVANCED_FACE('',(#589),#3199,.F.);
#3301=ADVANCED_FACE('',(#590),#3200,.F.);
#3302=ADVANCED_FACE('',(#591),#3201,.F.);
#3303=ADVANCED_FACE('',(#592),#3202,.F.);
#3304=ADVANCED_FACE('',(#593,#335,#336,#337,#338,#339,#340,#341,#342,#343,
#344,#345,#346,#347,#348,#349,#350,#351,#352,#353,#354,#355,#356,#357,#358,
#359,#360,#361,#362,#363,#364,#365,#366,#367,#368,#369,#370,#371,#372,#373,
#374,#375,#376),#3203,.F.);
#3305=ADVANCED_FACE('',(#594,#377),#475,.F.);
#3306=ADVANCED_FACE('',(#595,#378),#476,.T.);
#3307=ADVANCED_FACE('',(#596),#3204,.F.);
#3308=ADVANCED_FACE('',(#597,#379,#380,#381,#382,#383,#384,#385,#386,#387,
#388,#389,#390,#391,#392,#393,#394,#395,#396,#397,#398,#399,#400,#401,#402,
#403,#404,#405,#406,#407,#408,#409,#410,#411,#412,#413,#414,#415,#416,#417,
#418,#419,#420),#3205,.T.);
#3309=ADVANCED_FACE('',(#598,#421),#477,.T.);
#3310=ADVANCED_FACE('',(#599,#422),#478,.F.);
#3311=ADVANCED_FACE('',(#600),#3206,.T.);
#3312=ADVANCED_FACE('',(#601),#3207,.T.);
#3313=ADVANCED_FACE('',(#602,#423),#479,.T.);
#3314=ADVANCED_FACE('',(#603,#424),#480,.F.);
#3315=ADVANCED_FACE('',(#604),#3208,.F.);
#3316=ADVANCED_FACE('',(#605),#3209,.T.);
#3317=ADVANCED_FACE('',(#606,#425),#481,.T.);
#3318=ADVANCED_FACE('',(#607,#426),#482,.F.);
#3319=ADVANCED_FACE('',(#608),#3210,.F.);
#3320=ADVANCED_FACE('',(#609),#3211,.T.);
#3321=ADVANCED_FACE('',(#610,#427),#483,.T.);
#3322=ADVANCED_FACE('',(#611,#428),#484,.F.);
#3323=ADVANCED_FACE('',(#612),#3212,.F.);
#3324=ADVANCED_FACE('',(#613),#3213,.F.);
#3325=ADVANCED_FACE('',(#614),#3214,.F.);
#3326=ADVANCED_FACE('',(#615),#3215,.F.);
#3327=ADVANCED_FACE('',(#616),#3216,.F.);
#3328=ADVANCED_FACE('',(#617),#3217,.T.);
#3329=ADVANCED_FACE('',(#618,#429,#430,#431,#432,#433),#485,.T.);
#3330=ADVANCED_FACE('',(#619,#434,#435,#436,#437,#438),#486,.F.);
#3331=ADVANCED_FACE('',(#620),#3218,.F.);
#3332=ADVANCED_FACE('',(#621),#3219,.F.);
#3333=ADVANCED_FACE('',(#622),#3220,.F.);
#3334=ADVANCED_FACE('',(#623),#3221,.F.);
#3335=ADVANCED_FACE('',(#624),#3222,.F.);
#3336=ADVANCED_FACE('',(#625),#3223,.T.);
#3337=ADVANCED_FACE('',(#626,#439),#487,.F.);
#3338=ADVANCED_FACE('',(#627),#3224,.T.);
#3339=ADVANCED_FACE('',(#628,#440,#441,#442,#443,#444),#488,.T.);
#3340=ADVANCED_FACE('',(#629,#445,#446,#447,#448,#449),#489,.F.);
#3341=ADVANCED_FACE('',(#630),#490,.T.);
#3342=ADVANCED_FACE('',(#631),#68,.T.);
#3343=ADVANCED_FACE('',(#632),#3225,.T.);
#3344=ADVANCED_FACE('',(#633),#69,.T.);
#3345=ADVANCED_FACE('',(#634,#450),#491,.T.);
#3346=ADVANCED_FACE('',(#635),#70,.T.);
#3347=ADVANCED_FACE('',(#636),#3226,.T.);
#3348=ADVANCED_FACE('',(#637),#71,.T.);
#3349=ADVANCED_FACE('',(#638),#492,.T.);
#3350=ADVANCED_FACE('',(#639),#493,.F.);
#3351=ADVANCED_FACE('',(#640),#494,.F.);
#3352=ADVANCED_FACE('',(#641),#495,.F.);
#3353=ADVANCED_FACE('',(#642),#496,.F.);
#3354=ADVANCED_FACE('',(#643),#497,.F.);
#3355=ADVANCED_FACE('',(#644),#498,.F.);
#3356=ADVANCED_FACE('',(#645),#499,.F.);
#3357=ADVANCED_FACE('',(#646),#500,.F.);
#3358=ADVANCED_FACE('',(#647,#451),#501,.F.);
#3359=ADVANCED_FACE('',(#648,#452),#502,.T.);
#3360=ADVANCED_FACE('',(#649),#503,.T.);
#3361=ADVANCED_FACE('',(#650),#504,.T.);
#3362=ADVANCED_FACE('',(#651),#505,.T.);
#3363=ADVANCED_FACE('',(#652),#506,.T.);
#3364=ADVANCED_FACE('',(#653),#507,.T.);
#3365=ADVANCED_FACE('',(#654),#508,.T.);
#3366=ADVANCED_FACE('',(#655),#3227,.T.);
#3367=ADVANCED_FACE('',(#656,#453),#509,.T.);
#3368=ADVANCED_FACE('',(#657),#72,.T.);
#3369=ADVANCED_FACE('',(#658),#3228,.T.);
#3370=ADVANCED_FACE('',(#659),#73,.T.);
#3371=ADVANCED_FACE('',(#660,#454),#510,.T.);
#3372=ADVANCED_FACE('',(#661),#3229,.F.);
#3373=ADVANCED_FACE('',(#662,#455),#511,.F.);
#3374=ADVANCED_FACE('',(#663),#512,.T.);
#3375=ADVANCED_FACE('',(#664),#513,.T.);
#3376=ADVANCED_FACE('',(#665),#514,.T.);
#3377=ADVANCED_FACE('',(#666),#515,.T.);
#3378=ADVANCED_FACE('',(#667),#516,.T.);
#3379=ADVANCED_FACE('',(#668),#517,.T.);
#3380=ADVANCED_FACE('',(#669),#518,.T.);
#3381=ADVANCED_FACE('',(#670),#3230,.T.);
#3382=ADVANCED_FACE('',(#671),#519,.F.);
#3383=CLOSED_SHELL('',(#3231,#3232,#3233,#3234,#3235,#3236,#3237,#3238,
#3239,#3240,#3241,#3242,#3243,#3244,#3245,#3246,#3247,#3248,#3249,#3250,
#3251,#3252,#3253,#3254));
#3384=CLOSED_SHELL('',(#3255,#3256,#3257,#3258,#3259,#3260,#3261,#3262,
#3263,#3264,#3265,#3266,#3267,#3268,#3269,#3270,#3271,#3272,#3273,#3274,
#3275,#3276,#3277,#3278,#3279,#3280,#3281,#3282,#3283,#3284,#3285,#3286,
#3287,#3288,#3289,#3290,#3291,#3292,#3293,#3294,#3295,#3296,#3297,#3298,
#3299,#3300,#3301,#3302,#3303,#3304,#3305,#3306,#3307,#3308,#3309,#3310,
#3311,#3312,#3313,#3314));
#3385=CLOSED_SHELL('',(#3315,#3316,#3317,#3318));
#3386=CLOSED_SHELL('',(#3319,#3320,#3321,#3322));
#3387=CLOSED_SHELL('',(#3323,#3324,#3325,#3326,#3327,#3328,#3329,#3330));
#3388=CLOSED_SHELL('',(#3331,#3332,#3333,#3334,#3335,#3336,#3337,#3338,
#3339,#3340));
#3389=CLOSED_SHELL('',(#3341,#3342,#3343,#3344,#3345,#3346,#3347,#3348,
#3349));
#3390=CLOSED_SHELL('',(#3350,#3351,#3352,#3353,#3354,#3355,#3356,#3357));
#3391=CLOSED_SHELL('',(#3358,#3359,#3360,#3361,#3362,#3363,#3364,#3365,
#3366,#3367,#3368,#3369,#3370,#3371,#3372));
#3392=CLOSED_SHELL('',(#3373,#3374,#3375,#3376,#3377,#3378,#3379,#3380,
#3381,#3382));
#3393=DERIVED_UNIT_ELEMENT(#3411,1.);
#3394=DERIVED_UNIT_ELEMENT(#8866,-3.);
#3395=DERIVED_UNIT_ELEMENT(#3411,1.);
#3396=DERIVED_UNIT_ELEMENT(#8866,-3.);
#3397=DERIVED_UNIT_ELEMENT(#3411,1.);
#3398=DERIVED_UNIT_ELEMENT(#8866,-3.);
#3399=DERIVED_UNIT_ELEMENT(#3411,1.);
#3400=DERIVED_UNIT_ELEMENT(#8866,-3.);
#3401=DERIVED_UNIT_ELEMENT(#3411,1.);
#3402=DERIVED_UNIT_ELEMENT(#8866,-3.);
#3403=DERIVED_UNIT_ELEMENT(#3411,1.);
#3404=DERIVED_UNIT_ELEMENT(#8866,-3.);
#3405=DERIVED_UNIT_ELEMENT(#3411,1.);
#3406=DERIVED_UNIT_ELEMENT(#8866,-3.);
#3407=DERIVED_UNIT_ELEMENT(#3411,1.);
#3408=DERIVED_UNIT_ELEMENT(#8866,-3.);
#3409=DERIVED_UNIT_ELEMENT(#3411,1.);
#3410=DERIVED_UNIT_ELEMENT(#8866,-3.);
#3411=(
MASS_UNIT()
NAMED_UNIT(*)
SI_UNIT(.KILO.,.GRAM.)
);
#3412=DERIVED_UNIT((#3393,#3394));
#3413=DERIVED_UNIT((#3395,#3396));
#3414=DERIVED_UNIT((#3397,#3398));
#3415=DERIVED_UNIT((#3399,#3400));
#3416=DERIVED_UNIT((#3401,#3402));
#3417=DERIVED_UNIT((#3403,#3404));
#3418=DERIVED_UNIT((#3405,#3406));
#3419=DERIVED_UNIT((#3407,#3408));
#3420=DERIVED_UNIT((#3409,#3410));
#3421=MEASURE_REPRESENTATION_ITEM('density measure',
POSITIVE_RATIO_MEASURE(7850.),#3412);
#3422=MEASURE_REPRESENTATION_ITEM('density measure',
POSITIVE_RATIO_MEASURE(7850.),#3413);
#3423=MEASURE_REPRESENTATION_ITEM('density measure',
POSITIVE_RATIO_MEASURE(7850.),#3414);
#3424=MEASURE_REPRESENTATION_ITEM('density measure',
POSITIVE_RATIO_MEASURE(7850.),#3415);
#3425=MEASURE_REPRESENTATION_ITEM('density measure',
POSITIVE_RATIO_MEASURE(7850.),#3416);
#3426=MEASURE_REPRESENTATION_ITEM('density measure',
POSITIVE_RATIO_MEASURE(7850.),#3417);
#3427=MEASURE_REPRESENTATION_ITEM('density measure',
POSITIVE_RATIO_MEASURE(7850.),#3418);
#3428=MEASURE_REPRESENTATION_ITEM('density measure',
POSITIVE_RATIO_MEASURE(7850.),#3419);
#3429=MEASURE_REPRESENTATION_ITEM('density measure',
POSITIVE_RATIO_MEASURE(7850.),#3420);
#3430=PROPERTY_DEFINITION_REPRESENTATION(#3475,#3448);
#3431=PROPERTY_DEFINITION_REPRESENTATION(#3476,#3449);
#3432=PROPERTY_DEFINITION_REPRESENTATION(#3477,#3450);
#3433=PROPERTY_DEFINITION_REPRESENTATION(#3478,#3451);
#3434=PROPERTY_DEFINITION_REPRESENTATION(#3479,#3452);
#3435=PROPERTY_DEFINITION_REPRESENTATION(#3480,#3453);
#3436=PROPERTY_DEFINITION_REPRESENTATION(#3481,#3454);
#3437=PROPERTY_DEFINITION_REPRESENTATION(#3482,#3455);
#3438=PROPERTY_DEFINITION_REPRESENTATION(#3483,#3456);
#3439=PROPERTY_DEFINITION_REPRESENTATION(#3484,#3457);
#3440=PROPERTY_DEFINITION_REPRESENTATION(#3485,#3458);
#3441=PROPERTY_DEFINITION_REPRESENTATION(#3486,#3459);
#3442=PROPERTY_DEFINITION_REPRESENTATION(#3487,#3460);
#3443=PROPERTY_DEFINITION_REPRESENTATION(#3488,#3461);
#3444=PROPERTY_DEFINITION_REPRESENTATION(#3489,#3462);
#3445=PROPERTY_DEFINITION_REPRESENTATION(#3490,#3463);
#3446=PROPERTY_DEFINITION_REPRESENTATION(#3491,#3464);
#3447=PROPERTY_DEFINITION_REPRESENTATION(#3492,#3465);
#3448=REPRESENTATION('material name',(#3466),#8855);
#3449=REPRESENTATION('density',(#3421),#8855);
#3450=REPRESENTATION('material name',(#3467),#8856);
#3451=REPRESENTATION('density',(#3422),#8856);
#3452=REPRESENTATION('material name',(#3468),#8857);
#3453=REPRESENTATION('density',(#3423),#8857);
#3454=REPRESENTATION('material name',(#3469),#8858);
#3455=REPRESENTATION('density',(#3424),#8858);
#3456=REPRESENTATION('material name',(#3470),#8859);
#3457=REPRESENTATION('density',(#3425),#8859);
#3458=REPRESENTATION('material name',(#3471),#8860);
#3459=REPRESENTATION('density',(#3426),#8860);
#3460=REPRESENTATION('material name',(#3472),#8861);
#3461=REPRESENTATION('density',(#3427),#8861);
#3462=REPRESENTATION('material name',(#3473),#8862);
#3463=REPRESENTATION('density',(#3428),#8862);
#3464=REPRESENTATION('material name',(#3474),#8863);
#3465=REPRESENTATION('density',(#3429),#8863);
#3466=DESCRIPTIVE_REPRESENTATION_ITEM('Steel','Steel');
#3467=DESCRIPTIVE_REPRESENTATION_ITEM('Steel','Steel');
#3468=DESCRIPTIVE_REPRESENTATION_ITEM('Steel','Steel');
#3469=DESCRIPTIVE_REPRESENTATION_ITEM('Steel','Steel');
#3470=DESCRIPTIVE_REPRESENTATION_ITEM('Steel','Steel');
#3471=DESCRIPTIVE_REPRESENTATION_ITEM('Steel','Steel');
#3472=DESCRIPTIVE_REPRESENTATION_ITEM('Steel','Steel');
#3473=DESCRIPTIVE_REPRESENTATION_ITEM('Steel','Steel');
#3474=DESCRIPTIVE_REPRESENTATION_ITEM('Steel','Steel');
#3475=PROPERTY_DEFINITION('material property','material name',#8919);
#3476=PROPERTY_DEFINITION('material property','density of part',#8919);
#3477=PROPERTY_DEFINITION('material property','material name',#8920);
#3478=PROPERTY_DEFINITION('material property','density of part',#8920);
#3479=PROPERTY_DEFINITION('material property','material name',#8921);
#3480=PROPERTY_DEFINITION('material property','density of part',#8921);
#3481=PROPERTY_DEFINITION('material property','material name',#8922);
#3482=PROPERTY_DEFINITION('material property','density of part',#8922);
#3483=PROPERTY_DEFINITION('material property','material name',#8923);
#3484=PROPERTY_DEFINITION('material property','density of part',#8923);
#3485=PROPERTY_DEFINITION('material property','material name',#8924);
#3486=PROPERTY_DEFINITION('material property','density of part',#8924);
#3487=PROPERTY_DEFINITION('material property','material name',#8925);
#3488=PROPERTY_DEFINITION('material property','density of part',#8925);
#3489=PROPERTY_DEFINITION('material property','material name',#8926);
#3490=PROPERTY_DEFINITION('material property','density of part',#8926);
#3491=PROPERTY_DEFINITION('material property','material name',#8927);
#3492=PROPERTY_DEFINITION('material property','density of part',#8927);
#3493=AXIS2_PLACEMENT_3D('',#4490,#3771,#3772);
#3494=AXIS2_PLACEMENT_3D('',#4491,#3773,#3774);
#3495=AXIS2_PLACEMENT_3D('',#4492,#3775,#3776);
#3496=AXIS2_PLACEMENT_3D('',#4493,#3777,#3778);
#3497=AXIS2_PLACEMENT_3D('',#4495,#3779,#3780);
#3498=AXIS2_PLACEMENT_3D('',#4498,#3782,#3783);
#3499=AXIS2_PLACEMENT_3D('',#4499,#3784,#3785);
#3500=AXIS2_PLACEMENT_3D('',#4501,#3786,#3787);
#3501=AXIS2_PLACEMENT_3D('',#4504,#3789,#3790);
#3502=AXIS2_PLACEMENT_3D('',#4505,#3791,#3792);
#3503=AXIS2_PLACEMENT_3D('',#4507,#3793,#3794);
#3504=AXIS2_PLACEMENT_3D('',#4510,#3796,#3797);
#3505=AXIS2_PLACEMENT_3D('',#4511,#3798,#3799);
#3506=AXIS2_PLACEMENT_3D('',#4513,#3800,#3801);
#3507=AXIS2_PLACEMENT_3D('',#4516,#3803,#3804);
#3508=AXIS2_PLACEMENT_3D('',#4517,#3805,#3806);
#3509=AXIS2_PLACEMENT_3D('',#4520,#3807,#3808);
#3510=AXIS2_PLACEMENT_3D('',#4522,#3809,#3810);
#3511=AXIS2_PLACEMENT_3D('',#4524,#3811,#3812);
#3512=AXIS2_PLACEMENT_3D('',#4527,#3814,#3815);
#3513=AXIS2_PLACEMENT_3D('',#4528,#3816,#3817);
#3514=AXIS2_PLACEMENT_3D('',#4573,#3819,#3820);
#3515=AXIS2_PLACEMENT_3D('',#4574,#3821,#3822);
#3516=AXIS2_PLACEMENT_3D('',#4576,#3823,#3824);
#3517=AXIS2_PLACEMENT_3D('',#4577,#3825,#3826);
#3518=AXIS2_PLACEMENT_3D('',#4578,#3827,#3828);
#3519=AXIS2_PLACEMENT_3D('',#4592,#3829,#3830);
#3520=AXIS2_PLACEMENT_3D('',#4594,#3832,#3833);
#3521=AXIS2_PLACEMENT_3D('',#4595,#3834,#3835);
#3522=AXIS2_PLACEMENT_3D('',#4597,#3836,#3837);
#3523=AXIS2_PLACEMENT_3D('',#4599,#3838,#3839);
#3524=AXIS2_PLACEMENT_3D('',#4600,#3840,#3841);
#3525=AXIS2_PLACEMENT_3D('',#4601,#3842,#3843);
#3526=AXIS2_PLACEMENT_3D('',#4603,#3844,#3845);
#3527=AXIS2_PLACEMENT_3D('',#4607,#3847,#3848);
#3528=AXIS2_PLACEMENT_3D('',#4646,#3849,#3850);
#3529=AXIS2_PLACEMENT_3D('',#4647,#3851,#3852);
#3530=AXIS2_PLACEMENT_3D('',#4648,#3853,#3854);
#3531=AXIS2_PLACEMENT_3D('',#4649,#3855,#3856);
#3532=AXIS2_PLACEMENT_3D('',#4650,#3857,#3858);
#3533=AXIS2_PLACEMENT_3D('',#4652,#3859,#3860);
#3534=AXIS2_PLACEMENT_3D('',#4655,#3862,#3863);
#3535=AXIS2_PLACEMENT_3D('',#4656,#3864,#3865);
#3536=AXIS2_PLACEMENT_3D('',#4658,#3866,#3867);
#3537=AXIS2_PLACEMENT_3D('',#4659,#3868,#3869);
#3538=AXIS2_PLACEMENT_3D('',#4661,#3870,#3871);
#3539=AXIS2_PLACEMENT_3D('',#4664,#3873,#3874);
#3540=AXIS2_PLACEMENT_3D('',#4665,#3875,#3876);
#3541=AXIS2_PLACEMENT_3D('',#4666,#3877,#3878);
#3542=AXIS2_PLACEMENT_3D('',#4668,#3880,#3881);
#3543=AXIS2_PLACEMENT_3D('',#4670,#3882,#3883);
#3544=AXIS2_PLACEMENT_3D('',#4672,#3884,#3885);
#3545=AXIS2_PLACEMENT_3D('',#4673,#3886,#3887);
#3546=AXIS2_PLACEMENT_3D('',#4675,#3888,#3889);
#3547=AXIS2_PLACEMENT_3D('',#4677,#3891,#3892);
#3548=AXIS2_PLACEMENT_3D('',#4681,#3894,#3895);
#3549=AXIS2_PLACEMENT_3D('',#4683,#3896,#3897);
#3550=AXIS2_PLACEMENT_3D('',#4684,#3898,#3899);
#3551=AXIS2_PLACEMENT_3D('',#4685,#3900,#3901);
#3552=AXIS2_PLACEMENT_3D('',#4686,#3902,#3903);
#3553=AXIS2_PLACEMENT_3D('',#4688,#3904,#3905);
#3554=AXIS2_PLACEMENT_3D('',#4691,#3907,#3908);
#3555=AXIS2_PLACEMENT_3D('',#4692,#3909,#3910);
#3556=AXIS2_PLACEMENT_3D('',#4693,#3911,#3912);
#3557=AXIS2_PLACEMENT_3D('',#4694,#3913,#3914);
#3558=AXIS2_PLACEMENT_3D('',#4695,#3915,#3916);
#3559=AXIS2_PLACEMENT_3D('',#4773,#3918,#3919);
#3560=AXIS2_PLACEMENT_3D('',#4851,#3921,#3922);
#3561=AXIS2_PLACEMENT_3D('',#4929,#3924,#3925);
#3562=AXIS2_PLACEMENT_3D('',#5007,#3927,#3928);
#3563=AXIS2_PLACEMENT_3D('',#5085,#3930,#3931);
#3564=AXIS2_PLACEMENT_3D('',#5163,#3933,#3934);
#3565=AXIS2_PLACEMENT_3D('',#5241,#3936,#3937);
#3566=AXIS2_PLACEMENT_3D('',#5319,#3939,#3940);
#3567=AXIS2_PLACEMENT_3D('',#5397,#3942,#3943);
#3568=AXIS2_PLACEMENT_3D('',#5475,#3945,#3946);
#3569=AXIS2_PLACEMENT_3D('',#5553,#3948,#3949);
#3570=AXIS2_PLACEMENT_3D('',#5631,#3951,#3952);
#3571=AXIS2_PLACEMENT_3D('',#5709,#3954,#3955);
#3572=AXIS2_PLACEMENT_3D('',#5787,#3957,#3958);
#3573=AXIS2_PLACEMENT_3D('',#5865,#3960,#3961);
#3574=AXIS2_PLACEMENT_3D('',#5943,#3963,#3964);
#3575=AXIS2_PLACEMENT_3D('',#6021,#3966,#3967);
#3576=AXIS2_PLACEMENT_3D('',#6099,#3969,#3970);
#3577=AXIS2_PLACEMENT_3D('',#6177,#3972,#3973);
#3578=AXIS2_PLACEMENT_3D('',#6255,#3975,#3976);
#3579=AXIS2_PLACEMENT_3D('',#6333,#3978,#3979);
#3580=AXIS2_PLACEMENT_3D('',#6411,#3981,#3982);
#3581=AXIS2_PLACEMENT_3D('',#6489,#3984,#3985);
#3582=AXIS2_PLACEMENT_3D('',#6567,#3987,#3988);
#3583=AXIS2_PLACEMENT_3D('',#6645,#3990,#3991);
#3584=AXIS2_PLACEMENT_3D('',#6723,#3993,#3994);
#3585=AXIS2_PLACEMENT_3D('',#6801,#3996,#3997);
#3586=AXIS2_PLACEMENT_3D('',#6879,#3999,#4000);
#3587=AXIS2_PLACEMENT_3D('',#6957,#4002,#4003);
#3588=AXIS2_PLACEMENT_3D('',#7035,#4005,#4006);
#3589=AXIS2_PLACEMENT_3D('',#7113,#4008,#4009);
#3590=AXIS2_PLACEMENT_3D('',#7191,#4011,#4012);
#3591=AXIS2_PLACEMENT_3D('',#7269,#4014,#4015);
#3592=AXIS2_PLACEMENT_3D('',#7347,#4017,#4018);
#3593=AXIS2_PLACEMENT_3D('',#7425,#4020,#4021);
#3594=AXIS2_PLACEMENT_3D('',#7503,#4023,#4024);
#3595=AXIS2_PLACEMENT_3D('',#7587,#4026,#4027);
#3596=AXIS2_PLACEMENT_3D('',#7665,#4029,#4030);
#3597=AXIS2_PLACEMENT_3D('',#7749,#4032,#4033);
#3598=AXIS2_PLACEMENT_3D('',#7827,#4035,#4036);
#3599=AXIS2_PLACEMENT_3D('',#7911,#4038,#4039);
#3600=AXIS2_PLACEMENT_3D('',#7989,#4041,#4042);
#3601=AXIS2_PLACEMENT_3D('',#8073,#4044,#4045);
#3602=AXIS2_PLACEMENT_3D('',#8151,#4047,#4048);
#3603=AXIS2_PLACEMENT_3D('',#8235,#4050,#4051);
#3604=AXIS2_PLACEMENT_3D('',#8313,#4053,#4054);
#3605=AXIS2_PLACEMENT_3D('',#8397,#4056,#4057);
#3606=AXIS2_PLACEMENT_3D('',#8475,#4059,#4060);
#3607=AXIS2_PLACEMENT_3D('',#8477,#4061,#4062);
#3608=AXIS2_PLACEMENT_3D('',#8480,#4064,#4065);
#3609=AXIS2_PLACEMENT_3D('',#8481,#4066,#4067);
#3610=AXIS2_PLACEMENT_3D('',#8483,#4068,#4069);
#3611=AXIS2_PLACEMENT_3D('',#8492,#4077,#4078);
#3612=AXIS2_PLACEMENT_3D('',#8493,#4079,#4080);
#3613=AXIS2_PLACEMENT_3D('',#8494,#4081,#4082);
#3614=AXIS2_PLACEMENT_3D('',#8496,#4083,#4084);
#3615=AXIS2_PLACEMENT_3D('',#8497,#4085,#4086);
#3616=AXIS2_PLACEMENT_3D('',#8499,#4087,#4088);
#3617=AXIS2_PLACEMENT_3D('',#8501,#4090,#4091);
#3618=AXIS2_PLACEMENT_3D('',#8503,#4092,#4093);
#3619=AXIS2_PLACEMENT_3D('',#8512,#4101,#4102);
#3620=AXIS2_PLACEMENT_3D('',#8513,#4103,#4104);
#3621=AXIS2_PLACEMENT_3D('',#8514,#4105,#4106);
#3622=AXIS2_PLACEMENT_3D('',#8516,#4107,#4108);
#3623=AXIS2_PLACEMENT_3D('',#8518,#4109,#4110);
#3624=AXIS2_PLACEMENT_3D('',#8519,#4111,#4112);
#3625=AXIS2_PLACEMENT_3D('',#8521,#4113,#4114);
#3626=AXIS2_PLACEMENT_3D('',#8523,#4116,#4117);
#3627=AXIS2_PLACEMENT_3D('',#8526,#4119,#4120);
#3628=AXIS2_PLACEMENT_3D('',#8527,#4121,#4122);
#3629=AXIS2_PLACEMENT_3D('',#8528,#4123,#4124);
#3630=AXIS2_PLACEMENT_3D('',#8529,#4125,#4126);
#3631=AXIS2_PLACEMENT_3D('',#8530,#4127,#4128);
#3632=AXIS2_PLACEMENT_3D('',#8532,#4129,#4130);
#3633=AXIS2_PLACEMENT_3D('',#8535,#4132,#4133);
#3634=AXIS2_PLACEMENT_3D('',#8536,#4134,#4135);
#3635=AXIS2_PLACEMENT_3D('',#8538,#4136,#4137);
#3636=AXIS2_PLACEMENT_3D('',#8541,#4139,#4140);
#3637=AXIS2_PLACEMENT_3D('',#8542,#4141,#4142);
#3638=AXIS2_PLACEMENT_3D('',#8543,#4143,#4144);
#3639=AXIS2_PLACEMENT_3D('',#8544,#4145,#4146);
#3640=AXIS2_PLACEMENT_3D('',#8545,#4147,#4148);
#3641=AXIS2_PLACEMENT_3D('',#8547,#4149,#4150);
#3642=AXIS2_PLACEMENT_3D('',#8550,#4152,#4153);
#3643=AXIS2_PLACEMENT_3D('',#8551,#4154,#4155);
#3644=AXIS2_PLACEMENT_3D('',#8553,#4156,#4157);
#3645=AXIS2_PLACEMENT_3D('',#8556,#4159,#4160);
#3646=AXIS2_PLACEMENT_3D('',#8557,#4161,#4162);
#3647=AXIS2_PLACEMENT_3D('',#8558,#4163,#4164);
#3648=AXIS2_PLACEMENT_3D('',#8559,#4165,#4166);
#3649=AXIS2_PLACEMENT_3D('',#8560,#4167,#4168);
#3650=AXIS2_PLACEMENT_3D('',#8562,#4169,#4170);
#3651=AXIS2_PLACEMENT_3D('',#8565,#4172,#4173);
#3652=AXIS2_PLACEMENT_3D('',#8566,#4174,#4175);
#3653=AXIS2_PLACEMENT_3D('',#8568,#4176,#4177);
#3654=AXIS2_PLACEMENT_3D('',#8571,#4179,#4180);
#3655=AXIS2_PLACEMENT_3D('',#8572,#4181,#4182);
#3656=AXIS2_PLACEMENT_3D('',#8574,#4183,#4184);
#3657=AXIS2_PLACEMENT_3D('',#8577,#4186,#4187);
#3658=AXIS2_PLACEMENT_3D('',#8578,#4188,#4189);
#3659=AXIS2_PLACEMENT_3D('',#8580,#4190,#4191);
#3660=AXIS2_PLACEMENT_3D('',#8583,#4193,#4194);
#3661=AXIS2_PLACEMENT_3D('',#8584,#4195,#4196);
#3662=AXIS2_PLACEMENT_3D('',#8586,#4197,#4198);
#3663=AXIS2_PLACEMENT_3D('',#8589,#4200,#4201);
#3664=AXIS2_PLACEMENT_3D('',#8590,#4202,#4203);
#3665=AXIS2_PLACEMENT_3D('',#8592,#4204,#4205);
#3666=AXIS2_PLACEMENT_3D('',#8595,#4207,#4208);
#3667=AXIS2_PLACEMENT_3D('',#8596,#4209,#4210);
#3668=AXIS2_PLACEMENT_3D('',#8597,#4211,#4212);
#3669=AXIS2_PLACEMENT_3D('',#8598,#4213,#4214);
#3670=AXIS2_PLACEMENT_3D('',#8599,#4215,#4216);
#3671=AXIS2_PLACEMENT_3D('',#8601,#4217,#4218);
#3672=AXIS2_PLACEMENT_3D('',#8604,#4220,#4221);
#3673=AXIS2_PLACEMENT_3D('',#8605,#4222,#4223);
#3674=AXIS2_PLACEMENT_3D('',#8607,#4224,#4225);
#3675=AXIS2_PLACEMENT_3D('',#8610,#4227,#4228);
#3676=AXIS2_PLACEMENT_3D('',#8611,#4229,#4230);
#3677=AXIS2_PLACEMENT_3D('',#8613,#4231,#4232);
#3678=AXIS2_PLACEMENT_3D('',#8616,#4234,#4235);
#3679=AXIS2_PLACEMENT_3D('',#8617,#4236,#4237);
#3680=AXIS2_PLACEMENT_3D('',#8619,#4238,#4239);
#3681=AXIS2_PLACEMENT_3D('',#8622,#4241,#4242);
#3682=AXIS2_PLACEMENT_3D('',#8623,#4243,#4244);
#3683=AXIS2_PLACEMENT_3D('',#8625,#4245,#4246);
#3684=AXIS2_PLACEMENT_3D('',#8628,#4248,#4249);
#3685=AXIS2_PLACEMENT_3D('',#8629,#4250,#4251);
#3686=AXIS2_PLACEMENT_3D('',#8631,#4252,#4253);
#3687=AXIS2_PLACEMENT_3D('',#8634,#4255,#4256);
#3688=AXIS2_PLACEMENT_3D('',#8635,#4257,#4258);
#3689=AXIS2_PLACEMENT_3D('',#8636,#4259,#4260);
#3690=AXIS2_PLACEMENT_3D('',#8638,#4261,#4262);
#3691=AXIS2_PLACEMENT_3D('',#8641,#4264,#4265);
#3692=AXIS2_PLACEMENT_3D('',#8642,#4266,#4267);
#3693=AXIS2_PLACEMENT_3D('',#8643,#4268,#4269);
#3694=AXIS2_PLACEMENT_3D('',#8644,#4270,#4271);
#3695=AXIS2_PLACEMENT_3D('',#8645,#4272,#4273);
#3696=AXIS2_PLACEMENT_3D('',#8647,#4274,#4275);
#3697=AXIS2_PLACEMENT_3D('',#8648,#4276,#4277);
#3698=AXIS2_PLACEMENT_3D('',#8650,#4278,#4279);
#3699=AXIS2_PLACEMENT_3D('',#8652,#4281,#4282);
#3700=AXIS2_PLACEMENT_3D('',#8654,#4283,#4284);
#3701=AXIS2_PLACEMENT_3D('',#8656,#4286,#4287);
#3702=AXIS2_PLACEMENT_3D('',#8658,#4288,#4289);
#3703=AXIS2_PLACEMENT_3D('',#8660,#4291,#4292);
#3704=AXIS2_PLACEMENT_3D('',#8662,#4293,#4294);
#3705=AXIS2_PLACEMENT_3D('',#8663,#4295,#4296);
#3706=AXIS2_PLACEMENT_3D('',#8665,#4297,#4298);
#3707=AXIS2_PLACEMENT_3D('',#8667,#4300,#4301);
#3708=AXIS2_PLACEMENT_3D('',#8669,#4302,#4303);
#3709=AXIS2_PLACEMENT_3D('',#8671,#4305,#4306);
#3710=AXIS2_PLACEMENT_3D('',#8673,#4307,#4308);
#3711=AXIS2_PLACEMENT_3D('',#8675,#4310,#4311);
#3712=AXIS2_PLACEMENT_3D('',#8676,#4312,#4313);
#3713=AXIS2_PLACEMENT_3D('',#8685,#4318,#4319);
#3714=AXIS2_PLACEMENT_3D('',#8691,#4323,#4324);
#3715=AXIS2_PLACEMENT_3D('',#8697,#4328,#4329);
#3716=AXIS2_PLACEMENT_3D('',#8703,#4333,#4334);
#3717=AXIS2_PLACEMENT_3D('',#8709,#4338,#4339);
#3718=AXIS2_PLACEMENT_3D('',#8712,#4342,#4343);
#3719=AXIS2_PLACEMENT_3D('',#8713,#4344,#4345);
#3720=AXIS2_PLACEMENT_3D('',#8714,#4346,#4347);
#3721=AXIS2_PLACEMENT_3D('',#8715,#4348,#4349);
#3722=AXIS2_PLACEMENT_3D('',#8729,#4356,#4357);
#3723=AXIS2_PLACEMENT_3D('',#8730,#4358,#4359);
#3724=AXIS2_PLACEMENT_3D('',#8744,#4366,#4367);
#3725=AXIS2_PLACEMENT_3D('',#8745,#4368,#4369);
#3726=AXIS2_PLACEMENT_3D('',#8748,#4372,#4373);
#3727=AXIS2_PLACEMENT_3D('',#8750,#4375,#4376);
#3728=AXIS2_PLACEMENT_3D('',#8752,#4378,#4379);
#3729=AXIS2_PLACEMENT_3D('',#8754,#4381,#4382);
#3730=AXIS2_PLACEMENT_3D('',#8756,#4384,#4385);
#3731=AXIS2_PLACEMENT_3D('',#8757,#4386,#4387);
#3732=AXIS2_PLACEMENT_3D('',#8760,#4389,#4390);
#3733=AXIS2_PLACEMENT_3D('',#8761,#4391,#4392);
#3734=AXIS2_PLACEMENT_3D('',#8763,#4393,#4394);
#3735=AXIS2_PLACEMENT_3D('',#8765,#4395,#4396);
#3736=AXIS2_PLACEMENT_3D('',#8766,#4397,#4398);
#3737=AXIS2_PLACEMENT_3D('',#8768,#4400,#4401);
#3738=AXIS2_PLACEMENT_3D('',#8770,#4402,#4403);
#3739=AXIS2_PLACEMENT_3D('',#8772,#4405,#4406);
#3740=AXIS2_PLACEMENT_3D('',#8774,#4407,#4408);
#3741=AXIS2_PLACEMENT_3D('',#8776,#4410,#4411);
#3742=AXIS2_PLACEMENT_3D('',#8778,#4412,#4413);
#3743=AXIS2_PLACEMENT_3D('',#8779,#4414,#4415);
#3744=AXIS2_PLACEMENT_3D('',#8781,#4417,#4418);
#3745=AXIS2_PLACEMENT_3D('',#8782,#4419,#4420);
#3746=AXIS2_PLACEMENT_3D('',#8796,#4427,#4428);
#3747=AXIS2_PLACEMENT_3D('',#8797,#4429,#4430);
#3748=AXIS2_PLACEMENT_3D('',#8803,#4434,#4435);
#3749=AXIS2_PLACEMENT_3D('',#8807,#4438,#4439);
#3750=AXIS2_PLACEMENT_3D('',#8811,#4442,#4443);
#3751=AXIS2_PLACEMENT_3D('',#8815,#4446,#4447);
#3752=AXIS2_PLACEMENT_3D('',#8819,#4450,#4451);
#3753=AXIS2_PLACEMENT_3D('',#8821,#4453,#4454);
#3754=AXIS2_PLACEMENT_3D('',#8822,#4455,#4456);
#3755=AXIS2_PLACEMENT_3D('',#8825,#4458,#4459);
#3756=AXIS2_PLACEMENT_3D('',#8826,#4460,#4461);
#3757=AXIS2_PLACEMENT_3D('',#8827,#4462,#4463);
#3758=AXIS2_PLACEMENT_3D('',#8828,#4464,#4465);
#3759=AXIS2_PLACEMENT_3D('',#8829,#4466,#4467);
#3760=AXIS2_PLACEMENT_3D('',#8830,#4468,#4469);
#3761=AXIS2_PLACEMENT_3D('',#8831,#4470,#4471);
#3762=AXIS2_PLACEMENT_3D('',#8832,#4472,#4473);
#3763=AXIS2_PLACEMENT_3D('',#8833,#4474,#4475);
#3764=AXIS2_PLACEMENT_3D('',#8834,#4476,#4477);
#3765=AXIS2_PLACEMENT_3D('',#8835,#4478,#4479);
#3766=AXIS2_PLACEMENT_3D('',#8836,#4480,#4481);
#3767=AXIS2_PLACEMENT_3D('',#8837,#4482,#4483);
#3768=AXIS2_PLACEMENT_3D('',#8838,#4484,#4485);
#3769=AXIS2_PLACEMENT_3D('',#8839,#4486,#4487);
#3770=AXIS2_PLACEMENT_3D('',#8840,#4488,#4489);
#3771=DIRECTION('axis',(0.,0.,1.));
#3772=DIRECTION('refdir',(1.,0.,0.));
#3773=DIRECTION('axis',(0.,0.,1.));
#3774=DIRECTION('refdir',(1.,0.,0.));
#3775=DIRECTION('axis',(0.,0.,1.));
#3776=DIRECTION('refdir',(1.,0.,0.));
#3777=DIRECTION('center_axis',(0.707106781186548,0.,-0.707106781186547));
#3778=DIRECTION('ref_axis',(-0.707106781186547,0.,-0.707106781186548));
#3779=DIRECTION('center_axis',(0.707106781186548,0.,-0.707106781186547));
#3780=DIRECTION('ref_axis',(-0.707106781186547,0.,-0.707106781186548));
#3781=DIRECTION('',(0.707106781186548,0.,-0.707106781186547));
#3782=DIRECTION('center_axis',(-0.707106781186548,0.,0.707106781186547));
#3783=DIRECTION('ref_axis',(-0.707106781186547,0.,-0.707106781186548));
#3784=DIRECTION('center_axis',(0.707106781186548,0.,-0.707106781186547));
#3785=DIRECTION('ref_axis',(-0.707106781186547,0.,-0.707106781186548));
#3786=DIRECTION('center_axis',(0.707106781186548,0.,-0.707106781186547));
#3787=DIRECTION('ref_axis',(-0.707106781186547,0.,-0.707106781186548));
#3788=DIRECTION('',(0.707106781186548,0.,-0.707106781186547));
#3789=DIRECTION('center_axis',(-0.707106781186548,0.,0.707106781186547));
#3790=DIRECTION('ref_axis',(-0.707106781186547,0.,-0.707106781186548));
#3791=DIRECTION('center_axis',(0.707106781186548,0.,-0.707106781186547));
#3792=DIRECTION('ref_axis',(-0.707106781186547,0.,-0.707106781186548));
#3793=DIRECTION('center_axis',(0.707106781186548,0.,-0.707106781186547));
#3794=DIRECTION('ref_axis',(-0.707106781186547,0.,-0.707106781186548));
#3795=DIRECTION('',(0.707106781186548,0.,-0.707106781186547));
#3796=DIRECTION('center_axis',(-0.707106781186548,0.,0.707106781186547));
#3797=DIRECTION('ref_axis',(-0.707106781186547,0.,-0.707106781186548));
#3798=DIRECTION('center_axis',(0.707106781186548,0.,-0.707106781186547));
#3799=DIRECTION('ref_axis',(-0.707106781186547,0.,-0.707106781186548));
#3800=DIRECTION('center_axis',(0.707106781186548,0.,-0.707106781186547));
#3801=DIRECTION('ref_axis',(-0.707106781186547,0.,-0.707106781186548));
#3802=DIRECTION('',(0.707106781186548,0.,-0.707106781186547));
#3803=DIRECTION('center_axis',(-0.707106781186548,0.,0.707106781186547));
#3804=DIRECTION('ref_axis',(-0.707106781186547,0.,-0.707106781186548));
#3805=DIRECTION('center_axis',(0.707106781186548,0.,-0.707106781186547));
#3806=DIRECTION('ref_axis',(-0.707106781186547,0.,-0.707106781186548));
#3807=DIRECTION('center_axis',(0.707106781186548,0.,-0.707106781186547));
#3808=DIRECTION('ref_axis',(-0.707106781186547,0.,-0.707106781186548));
#3809=DIRECTION('center_axis',(0.707106781186548,0.,-0.707106781186547));
#3810=DIRECTION('ref_axis',(-0.707106781186547,0.,-0.707106781186548));
#3811=DIRECTION('center_axis',(0.707106781186548,0.,-0.707106781186547));
#3812=DIRECTION('ref_axis',(-0.707106781186547,0.,-0.707106781186548));
#3813=DIRECTION('',(0.,1.,0.));
#3814=DIRECTION('center_axis',(0.707106781186548,0.,-0.707106781186547));
#3815=DIRECTION('ref_axis',(-0.707106781186547,0.,-0.707106781186548));
#3816=DIRECTION('center_axis',(0.707106781186548,0.,-0.707106781186547));
#3817=DIRECTION('ref_axis',(-0.707106781186547,0.,-0.707106781186548));
#3818=DIRECTION('',(0.707106781186548,0.,-0.707106781186547));
#3819=DIRECTION('center_axis',(-0.707106781186548,0.,0.707106781186547));
#3820=DIRECTION('ref_axis',(-0.707106781186547,0.,-0.707106781186548));
#3821=DIRECTION('center_axis',(1.,0.,0.));
#3822=DIRECTION('ref_axis',(0.,0.,-1.));
#3823=DIRECTION('center_axis',(1.,0.,0.));
#3824=DIRECTION('ref_axis',(0.,0.,-1.));
#3825=DIRECTION('center_axis',(1.,0.,0.));
#3826=DIRECTION('ref_axis',(0.,0.,-1.));
#3827=DIRECTION('center_axis',(0.707106781186548,0.,-0.707106781186547));
#3828=DIRECTION('ref_axis',(-0.707106781186547,0.,-0.707106781186548));
#3829=DIRECTION('center_axis',(0.707106781186548,0.,-0.707106781186547));
#3830=DIRECTION('ref_axis',(-0.707106781186547,0.,-0.707106781186548));
#3831=DIRECTION('',(0.707106781186548,0.,-0.707106781186547));
#3832=DIRECTION('center_axis',(0.707106781186548,0.,-0.707106781186547));
#3833=DIRECTION('ref_axis',(-0.707106781186547,0.,-0.707106781186548));
#3834=DIRECTION('center_axis',(0.707106781186548,0.,-0.707106781186547));
#3835=DIRECTION('ref_axis',(-0.707106781186547,0.,-0.707106781186548));
#3836=DIRECTION('center_axis',(0.707106781186548,0.,-0.707106781186547));
#3837=DIRECTION('ref_axis',(-0.707106781186547,0.,-0.707106781186548));
#3838=DIRECTION('center_axis',(0.707106781186548,0.,-0.707106781186547));
#3839=DIRECTION('ref_axis',(-0.707106781186547,0.,-0.707106781186548));
#3840=DIRECTION('center_axis',(0.707106781186548,0.,-0.707106781186547));
#3841=DIRECTION('ref_axis',(-0.707106781186547,0.,-0.707106781186548));
#3842=DIRECTION('center_axis',(1.,0.,0.));
#3843=DIRECTION('ref_axis',(0.,0.,-1.));
#3844=DIRECTION('center_axis',(-1.,0.,0.));
#3845=DIRECTION('ref_axis',(0.,0.,-1.));
#3846=DIRECTION('',(1.,0.,0.));
#3847=DIRECTION('center_axis',(0.707106781186548,0.,-0.707106781186547));
#3848=DIRECTION('ref_axis',(-0.707106781186547,0.,-0.707106781186548));
#3849=DIRECTION('center_axis',(0.707106781186548,0.,-0.707106781186547));
#3850=DIRECTION('ref_axis',(-0.707106781186547,0.,-0.707106781186548));
#3851=DIRECTION('center_axis',(0.707106781186548,0.,-0.707106781186547));
#3852=DIRECTION('ref_axis',(-0.707106781186547,0.,-0.707106781186548));
#3853=DIRECTION('center_axis',(0.707106781186548,0.,-0.707106781186547));
#3854=DIRECTION('ref_axis',(-0.707106781186547,0.,-0.707106781186548));
#3855=DIRECTION('center_axis',(0.707106781186548,0.,-0.707106781186547));
#3856=DIRECTION('ref_axis',(0.707106781186547,5.66553889764798E-16,0.707106781186548));
#3857=DIRECTION('center_axis',(1.,0.,0.));
#3858=DIRECTION('ref_axis',(0.,0.,-1.));
#3859=DIRECTION('center_axis',(1.,0.,0.));
#3860=DIRECTION('ref_axis',(0.,0.,-1.));
#3861=DIRECTION('',(1.,0.,0.));
#3862=DIRECTION('center_axis',(-1.,0.,0.));
#3863=DIRECTION('ref_axis',(0.,0.,-1.));
#3864=DIRECTION('center_axis',(1.,0.,0.));
#3865=DIRECTION('ref_axis',(0.,0.,-1.));
#3866=DIRECTION('center_axis',(1.,0.,0.));
#3867=DIRECTION('ref_axis',(0.,0.,-1.));
#3868=DIRECTION('center_axis',(1.,0.,0.));
#3869=DIRECTION('ref_axis',(0.,0.,-1.));
#3870=DIRECTION('center_axis',(1.,0.,0.));
#3871=DIRECTION('ref_axis',(0.,0.,-1.));
#3872=DIRECTION('',(1.,0.,0.));
#3873=DIRECTION('center_axis',(1.,0.,0.));
#3874=DIRECTION('ref_axis',(0.,0.,-1.));
#3875=DIRECTION('center_axis',(1.,0.,0.));
#3876=DIRECTION('ref_axis',(0.,0.,-1.));
#3877=DIRECTION('center_axis',(1.,0.,0.));
#3878=DIRECTION('ref_axis',(0.,0.,-1.));
#3879=DIRECTION('',(1.,0.,0.));
#3880=DIRECTION('center_axis',(0.707106781186548,0.,-0.707106781186547));
#3881=DIRECTION('ref_axis',(-0.707106781186547,0.,-0.707106781186548));
#3882=DIRECTION('center_axis',(0.707106781186548,0.,-0.707106781186547));
#3883=DIRECTION('ref_axis',(-0.707106781186547,0.,-0.707106781186548));
#3884=DIRECTION('center_axis',(-0.707106781186548,0.,0.707106781186547));
#3885=DIRECTION('ref_axis',(-0.707106781186547,0.,-0.707106781186548));
#3886=DIRECTION('center_axis',(0.707106781186548,0.,-0.707106781186547));
#3887=DIRECTION('ref_axis',(-0.707106781186547,0.,-0.707106781186548));
#3888=DIRECTION('center_axis',(0.707106781186548,0.,-0.707106781186547));
#3889=DIRECTION('ref_axis',(-0.707106781186547,0.,-0.707106781186548));
#3890=DIRECTION('',(-0.707106781186548,0.,0.707106781186547));
#3891=DIRECTION('center_axis',(0.707106781186548,0.,-0.707106781186547));
#3892=DIRECTION('ref_axis',(-0.707106781186547,0.,-0.707106781186548));
#3893=DIRECTION('',(-0.707106781186548,0.,0.707106781186547));
#3894=DIRECTION('center_axis',(0.38268343236509,0.,0.923879532511287));
#3895=DIRECTION('ref_axis',(-0.923879532511287,0.,0.38268343236509));
#3896=DIRECTION('center_axis',(-0.923879532511287,0.,0.38268343236509));
#3897=DIRECTION('ref_axis',(-0.38268343236509,0.,-0.923879532511287));
#3898=DIRECTION('center_axis',(0.38268343236509,0.,0.923879532511287));
#3899=DIRECTION('ref_axis',(-0.923879532511287,0.,0.38268343236509));
#3900=DIRECTION('center_axis',(0.707106781186548,0.,-0.707106781186547));
#3901=DIRECTION('ref_axis',(-0.707106781186547,0.,-0.707106781186548));
#3902=DIRECTION('center_axis',(1.,0.,0.));
#3903=DIRECTION('ref_axis',(0.,0.,-1.));
#3904=DIRECTION('center_axis',(1.,0.,0.));
#3905=DIRECTION('ref_axis',(0.,0.,-1.));
#3906=DIRECTION('',(-1.,0.,0.));
#3907=DIRECTION('center_axis',(1.,0.,0.));
#3908=DIRECTION('ref_axis',(0.,0.,-1.));
#3909=DIRECTION('center_axis',(1.,0.,0.));
#3910=DIRECTION('ref_axis',(0.,0.,-1.));
#3911=DIRECTION('center_axis',(1.,0.,0.));
#3912=DIRECTION('ref_axis',(0.,0.,-1.));
#3913=DIRECTION('axis',(0.,0.,1.));
#3914=DIRECTION('refdir',(1.,0.,0.));
#3915=DIRECTION('center_axis',(0.5,0.707106781186548,0.5));
#3916=DIRECTION('ref_axis',(-0.707106781186548,0.,0.707106781186547));
#3917=DIRECTION('',(0.5,0.707106781186548,0.5));
#3918=DIRECTION('center_axis',(0.5,0.707106781186548,0.5));
#3919=DIRECTION('ref_axis',(-0.707106781186548,0.,0.707106781186547));
#3920=DIRECTION('',(0.5,0.707106781186548,0.5));
#3921=DIRECTION('center_axis',(0.5,0.707106781186548,0.5));
#3922=DIRECTION('ref_axis',(-0.707106781186548,0.,0.707106781186547));
#3923=DIRECTION('',(0.5,0.707106781186548,0.5));
#3924=DIRECTION('center_axis',(0.5,0.707106781186548,0.5));
#3925=DIRECTION('ref_axis',(-0.707106781186548,0.,0.707106781186547));
#3926=DIRECTION('',(0.5,0.707106781186548,0.5));
#3927=DIRECTION('center_axis',(0.5,0.707106781186548,0.5));
#3928=DIRECTION('ref_axis',(-0.707106781186548,0.,0.707106781186547));
#3929=DIRECTION('',(0.5,0.707106781186548,0.5));
#3930=DIRECTION('center_axis',(0.5,0.707106781186548,0.5));
#3931=DIRECTION('ref_axis',(-0.707106781186548,0.,0.707106781186547));
#3932=DIRECTION('',(0.5,0.707106781186548,0.5));
#3933=DIRECTION('center_axis',(0.5,0.707106781186548,0.5));
#3934=DIRECTION('ref_axis',(-0.707106781186548,0.,0.707106781186547));
#3935=DIRECTION('',(0.5,0.707106781186548,0.5));
#3936=DIRECTION('center_axis',(0.5,0.707106781186548,0.5));
#3937=DIRECTION('ref_axis',(-0.707106781186548,0.,0.707106781186547));
#3938=DIRECTION('',(0.5,0.707106781186548,0.5));
#3939=DIRECTION('center_axis',(0.5,0.707106781186548,0.5));
#3940=DIRECTION('ref_axis',(-0.707106781186548,0.,0.707106781186547));
#3941=DIRECTION('',(0.5,0.707106781186548,0.5));
#3942=DIRECTION('center_axis',(0.5,0.707106781186548,0.5));
#3943=DIRECTION('ref_axis',(-0.707106781186548,0.,0.707106781186547));
#3944=DIRECTION('',(0.5,0.707106781186548,0.5));
#3945=DIRECTION('center_axis',(0.5,0.707106781186548,0.5));
#3946=DIRECTION('ref_axis',(-0.707106781186548,0.,0.707106781186547));
#3947=DIRECTION('',(0.5,0.707106781186548,0.5));
#3948=DIRECTION('center_axis',(0.5,0.707106781186548,0.5));
#3949=DIRECTION('ref_axis',(-0.707106781186548,0.,0.707106781186547));
#3950=DIRECTION('',(0.5,0.707106781186548,0.5));
#3951=DIRECTION('center_axis',(-1.57009245868377E-16,1.,-1.57009245868378E-16));
#3952=DIRECTION('ref_axis',(-0.707106781186548,0.,0.707106781186547));
#3953=DIRECTION('',(-1.57009245868377E-16,1.,-1.57009245868378E-16));
#3954=DIRECTION('center_axis',(-1.57009245868377E-16,1.,-1.57009245868378E-16));
#3955=DIRECTION('ref_axis',(-0.707106781186548,0.,0.707106781186547));
#3956=DIRECTION('',(-1.57009245868377E-16,1.,-1.57009245868378E-16));
#3957=DIRECTION('center_axis',(-1.57009245868377E-16,1.,-1.57009245868378E-16));
#3958=DIRECTION('ref_axis',(-0.707106781186548,0.,0.707106781186547));
#3959=DIRECTION('',(-1.57009245868377E-16,1.,-1.57009245868378E-16));
#3960=DIRECTION('center_axis',(-1.57009245868377E-16,1.,-1.57009245868378E-16));
#3961=DIRECTION('ref_axis',(-0.707106781186548,0.,0.707106781186547));
#3962=DIRECTION('',(-1.57009245868377E-16,1.,-1.57009245868378E-16));
#3963=DIRECTION('center_axis',(-1.57009245868377E-16,1.,-1.57009245868378E-16));
#3964=DIRECTION('ref_axis',(-0.707106781186548,0.,0.707106781186547));
#3965=DIRECTION('',(-1.57009245868377E-16,1.,-1.57009245868378E-16));
#3966=DIRECTION('center_axis',(-1.57009245868377E-16,1.,-1.57009245868378E-16));
#3967=DIRECTION('ref_axis',(-0.707106781186548,0.,0.707106781186547));
#3968=DIRECTION('',(-1.57009245868377E-16,1.,-1.57009245868378E-16));
#3969=DIRECTION('center_axis',(-1.57009245868377E-16,1.,-1.57009245868378E-16));
#3970=DIRECTION('ref_axis',(-0.707106781186548,0.,0.707106781186547));
#3971=DIRECTION('',(-1.57009245868377E-16,1.,-1.57009245868378E-16));
#3972=DIRECTION('center_axis',(-1.57009245868377E-16,1.,-1.57009245868378E-16));
#3973=DIRECTION('ref_axis',(-0.707106781186548,0.,0.707106781186547));
#3974=DIRECTION('',(-1.57009245868377E-16,1.,-1.57009245868378E-16));
#3975=DIRECTION('center_axis',(-1.57009245868377E-16,1.,-1.57009245868378E-16));
#3976=DIRECTION('ref_axis',(-0.707106781186548,0.,0.707106781186547));
#3977=DIRECTION('',(-1.57009245868377E-16,1.,-1.57009245868378E-16));
#3978=DIRECTION('center_axis',(-1.57009245868377E-16,1.,-1.57009245868378E-16));
#3979=DIRECTION('ref_axis',(-0.707106781186548,0.,0.707106781186547));
#3980=DIRECTION('',(-1.57009245868377E-16,1.,-1.57009245868378E-16));
#3981=DIRECTION('center_axis',(-1.57009245868377E-16,1.,-1.57009245868378E-16));
#3982=DIRECTION('ref_axis',(-0.707106781186548,0.,0.707106781186547));
#3983=DIRECTION('',(-1.57009245868377E-16,1.,-1.57009245868378E-16));
#3984=DIRECTION('center_axis',(-1.57009245868377E-16,1.,-1.57009245868378E-16));
#3985=DIRECTION('ref_axis',(-0.707106781186548,0.,0.707106781186547));
#3986=DIRECTION('',(-1.57009245868377E-16,1.,-1.57009245868378E-16));
#3987=DIRECTION('center_axis',(-0.5,0.707106781186548,-0.5));
#3988=DIRECTION('ref_axis',(-0.707106781186548,0.,0.707106781186547));
#3989=DIRECTION('',(-0.5,0.707106781186548,-0.5));
#3990=DIRECTION('center_axis',(-0.5,0.707106781186548,-0.5));
#3991=DIRECTION('ref_axis',(-0.707106781186548,0.,0.707106781186547));
#3992=DIRECTION('',(-0.5,0.707106781186548,-0.5));
#3993=DIRECTION('center_axis',(-0.5,0.707106781186548,-0.5));
#3994=DIRECTION('ref_axis',(-0.707106781186548,0.,0.707106781186547));
#3995=DIRECTION('',(-0.5,0.707106781186548,-0.5));
#3996=DIRECTION('center_axis',(-0.5,0.707106781186548,-0.5));
#3997=DIRECTION('ref_axis',(-0.707106781186548,0.,0.707106781186547));
#3998=DIRECTION('',(-0.5,0.707106781186548,-0.5));
#3999=DIRECTION('center_axis',(-0.5,0.707106781186548,-0.5));
#4000=DIRECTION('ref_axis',(-0.707106781186548,0.,0.707106781186547));
#4001=DIRECTION('',(-0.5,0.707106781186547,-0.5));
#4002=DIRECTION('center_axis',(-0.5,0.707106781186548,-0.5));
#4003=DIRECTION('ref_axis',(-0.707106781186548,0.,0.707106781186547));
#4004=DIRECTION('',(-0.5,0.707106781186547,-0.5));
#4005=DIRECTION('center_axis',(-0.5,0.707106781186548,-0.5));
#4006=DIRECTION('ref_axis',(-0.707106781186548,0.,0.707106781186547));
#4007=DIRECTION('',(-0.5,0.707106781186547,-0.5));
#4008=DIRECTION('center_axis',(-0.5,0.707106781186548,-0.5));
#4009=DIRECTION('ref_axis',(-0.707106781186548,0.,0.707106781186547));
#4010=DIRECTION('',(-0.5,0.707106781186547,-0.5));
#4011=DIRECTION('center_axis',(-0.5,0.707106781186548,-0.5));
#4012=DIRECTION('ref_axis',(-0.707106781186548,0.,0.707106781186547));
#4013=DIRECTION('',(-0.5,0.707106781186547,-0.5));
#4014=DIRECTION('center_axis',(-0.5,0.707106781186548,-0.5));
#4015=DIRECTION('ref_axis',(-0.707106781186548,0.,0.707106781186547));
#4016=DIRECTION('',(-0.5,0.707106781186547,-0.5));
#4017=DIRECTION('center_axis',(-0.5,0.707106781186548,-0.5));
#4018=DIRECTION('ref_axis',(-0.707106781186548,0.,0.707106781186547));
#4019=DIRECTION('',(-0.5,0.707106781186548,-0.5));
#4020=DIRECTION('center_axis',(-0.5,0.707106781186548,-0.5));
#4021=DIRECTION('ref_axis',(-0.707106781186548,0.,0.707106781186547));
#4022=DIRECTION('',(-0.5,0.707106781186548,-0.5));
#4023=DIRECTION('center_axis',(-0.707106781186547,0.,-0.707106781186548));
#4024=DIRECTION('ref_axis',(-0.707106781186548,0.,0.707106781186547));
#4025=DIRECTION('',(-0.707106781186547,0.,-0.707106781186548));
#4026=DIRECTION('center_axis',(-0.707106781186547,0.,-0.707106781186548));
#4027=DIRECTION('ref_axis',(-0.707106781186548,0.,0.707106781186547));
#4028=DIRECTION('',(-0.707106781186547,0.,-0.707106781186548));
#4029=DIRECTION('center_axis',(-0.707106781186547,0.,-0.707106781186548));
#4030=DIRECTION('ref_axis',(-0.707106781186548,0.,0.707106781186547));
#4031=DIRECTION('',(-0.707106781186547,0.,-0.707106781186548));
#4032=DIRECTION('center_axis',(-0.707106781186547,0.,-0.707106781186548));
#4033=DIRECTION('ref_axis',(-0.707106781186548,0.,0.707106781186547));
#4034=DIRECTION('',(-0.707106781186547,0.,-0.707106781186548));
#4035=DIRECTION('center_axis',(-0.707106781186547,0.,-0.707106781186548));
#4036=DIRECTION('ref_axis',(-0.707106781186548,0.,0.707106781186547));
#4037=DIRECTION('',(-0.707106781186547,0.,-0.707106781186548));
#4038=DIRECTION('center_axis',(-0.707106781186547,0.,-0.707106781186548));
#4039=DIRECTION('ref_axis',(-0.707106781186548,0.,0.707106781186547));
#4040=DIRECTION('',(-0.707106781186547,0.,-0.707106781186548));
#4041=DIRECTION('center_axis',(-0.707106781186547,0.,-0.707106781186548));
#4042=DIRECTION('ref_axis',(-0.707106781186548,0.,0.707106781186547));
#4043=DIRECTION('',(-0.707106781186547,0.,-0.707106781186548));
#4044=DIRECTION('center_axis',(-0.707106781186547,0.,-0.707106781186548));
#4045=DIRECTION('ref_axis',(-0.707106781186548,0.,0.707106781186547));
#4046=DIRECTION('',(-0.707106781186547,0.,-0.707106781186548));
#4047=DIRECTION('center_axis',(-0.707106781186547,0.,-0.707106781186548));
#4048=DIRECTION('ref_axis',(-0.707106781186548,0.,0.707106781186547));
#4049=DIRECTION('',(-0.707106781186547,0.,-0.707106781186548));
#4050=DIRECTION('center_axis',(-0.707106781186547,0.,-0.707106781186548));
#4051=DIRECTION('ref_axis',(-0.707106781186548,0.,0.707106781186547));
#4052=DIRECTION('',(-0.707106781186547,0.,-0.707106781186548));
#4053=DIRECTION('center_axis',(-0.707106781186547,0.,-0.707106781186548));
#4054=DIRECTION('ref_axis',(-0.707106781186548,0.,0.707106781186547));
#4055=DIRECTION('',(-0.707106781186547,0.,-0.707106781186548));
#4056=DIRECTION('center_axis',(-0.707106781186547,0.,-0.707106781186548));
#4057=DIRECTION('ref_axis',(-0.707106781186548,0.,0.707106781186547));
#4058=DIRECTION('',(-0.707106781186547,0.,-0.707106781186548));
#4059=DIRECTION('center_axis',(0.707106781186548,0.,-0.707106781186547));
#4060=DIRECTION('ref_axis',(-0.707106781186547,0.,-0.707106781186548));
#4061=DIRECTION('center_axis',(0.707106781186548,0.,-0.707106781186547));
#4062=DIRECTION('ref_axis',(-0.707106781186547,0.,-0.707106781186548));
#4063=DIRECTION('',(0.707106781186548,0.,-0.707106781186547));
#4064=DIRECTION('center_axis',(-0.707106781186548,0.,0.707106781186547));
#4065=DIRECTION('ref_axis',(-0.707106781186547,0.,-0.707106781186548));
#4066=DIRECTION('center_axis',(0.707106781186548,0.,-0.707106781186547));
#4067=DIRECTION('ref_axis',(-0.707106781186547,0.,-0.707106781186548));
#4068=DIRECTION('center_axis',(0.707106781186548,0.,-0.707106781186547));
#4069=DIRECTION('ref_axis',(-0.707106781186547,0.,-0.707106781186548));
#4070=DIRECTION('',(0.707106781186548,0.,-0.707106781186547));
#4071=DIRECTION('',(0.707106781186548,0.,-0.707106781186547));
#4072=DIRECTION('',(0.707106781186548,0.,-0.707106781186547));
#4073=DIRECTION('',(0.707106781186548,0.,-0.707106781186547));
#4074=DIRECTION('',(0.707106781186548,0.,-0.707106781186547));
#4075=DIRECTION('',(0.707106781186548,0.,-0.707106781186547));
#4076=DIRECTION('',(0.707106781186548,0.,-0.707106781186547));
#4077=DIRECTION('center_axis',(0.707106781186548,0.,-0.707106781186547));
#4078=DIRECTION('ref_axis',(-0.707106781186547,0.,-0.707106781186548));
#4079=DIRECTION('center_axis',(0.707106781186548,0.,-0.707106781186547));
#4080=DIRECTION('ref_axis',(-0.707106781186547,0.,-0.707106781186548));
#4081=DIRECTION('center_axis',(0.707106781186548,0.,-0.707106781186547));
#4082=DIRECTION('ref_axis',(-0.707106781186547,0.,-0.707106781186548));
#4083=DIRECTION('center_axis',(0.707106781186548,0.,-0.707106781186547));
#4084=DIRECTION('ref_axis',(-0.707106781186547,0.,-0.707106781186548));
#4085=DIRECTION('center_axis',(0.707106781186548,0.,-0.707106781186547));
#4086=DIRECTION('ref_axis',(-0.707106781186547,0.,-0.707106781186548));
#4087=DIRECTION('center_axis',(0.707106781186548,0.,-0.707106781186547));
#4088=DIRECTION('ref_axis',(-0.707106781186547,0.,-0.707106781186548));
#4089=DIRECTION('',(0.707106781186548,0.,-0.707106781186547));
#4090=DIRECTION('center_axis',(0.707106781186548,0.,-0.707106781186547));
#4091=DIRECTION('ref_axis',(-0.707106781186547,0.,-0.707106781186548));
#4092=DIRECTION('center_axis',(0.707106781186548,0.,-0.707106781186547));
#4093=DIRECTION('ref_axis',(-0.707106781186547,0.,-0.707106781186548));
#4094=DIRECTION('',(-0.707106781186548,0.,0.707106781186547));
#4095=DIRECTION('',(-0.707106781186548,0.,0.707106781186547));
#4096=DIRECTION('',(-0.707106781186548,0.,0.707106781186547));
#4097=DIRECTION('',(-0.707106781186548,0.,0.707106781186547));
#4098=DIRECTION('',(-0.707106781186548,0.,0.707106781186547));
#4099=DIRECTION('',(-0.707106781186548,0.,0.707106781186547));
#4100=DIRECTION('',(-0.707106781186548,0.,0.707106781186547));
#4101=DIRECTION('center_axis',(-0.707106781186548,0.,0.707106781186547));
#4102=DIRECTION('ref_axis',(-0.707106781186547,0.,-0.707106781186548));
#4103=DIRECTION('center_axis',(0.707106781186548,0.,-0.707106781186547));
#4104=DIRECTION('ref_axis',(-0.707106781186547,0.,-0.707106781186548));
#4105=DIRECTION('center_axis',(0.707106781186548,0.,-0.707106781186547));
#4106=DIRECTION('ref_axis',(-0.707106781186547,0.,-0.707106781186548));
#4107=DIRECTION('center_axis',(0.707106781186548,0.,-0.707106781186547));
#4108=DIRECTION('ref_axis',(-0.707106781186547,0.,-0.707106781186548));
#4109=DIRECTION('center_axis',(-0.707106781186548,0.,0.707106781186547));
#4110=DIRECTION('ref_axis',(-0.707106781186547,0.,-0.707106781186548));
#4111=DIRECTION('center_axis',(0.707106781186548,0.,-0.707106781186547));
#4112=DIRECTION('ref_axis',(-0.707106781186547,0.,-0.707106781186548));
#4113=DIRECTION('center_axis',(0.707106781186548,0.,-0.707106781186547));
#4114=DIRECTION('ref_axis',(-0.707106781186547,0.,-0.707106781186548));
#4115=DIRECTION('',(-0.707106781186548,0.,0.707106781186547));
#4116=DIRECTION('center_axis',(0.707106781186548,0.,-0.707106781186547));
#4117=DIRECTION('ref_axis',(-0.707106781186547,0.,-0.707106781186548));
#4118=DIRECTION('',(-0.707106781186548,0.,0.707106781186547));
#4119=DIRECTION('center_axis',(0.707106781186548,0.,-0.707106781186547));
#4120=DIRECTION('ref_axis',(-0.707106781186547,0.,-0.707106781186548));
#4121=DIRECTION('center_axis',(0.707106781186548,0.,-0.707106781186547));
#4122=DIRECTION('ref_axis',(-0.707106781186547,0.,-0.707106781186548));
#4123=DIRECTION('center_axis',(0.707106781186548,0.,-0.707106781186547));
#4124=DIRECTION('ref_axis',(-0.707106781186547,0.,-0.707106781186548));
#4125=DIRECTION('axis',(0.,0.,1.));
#4126=DIRECTION('refdir',(1.,0.,0.));
#4127=DIRECTION('center_axis',(0.707106781186548,0.,-0.707106781186547));
#4128=DIRECTION('ref_axis',(-0.707106781186547,0.,-0.707106781186548));
#4129=DIRECTION('center_axis',(-0.707106781186548,0.,0.707106781186547));
#4130=DIRECTION('ref_axis',(-0.707106781186547,0.,-0.707106781186548));
#4131=DIRECTION('',(-0.707106781186548,0.,0.707106781186547));
#4132=DIRECTION('center_axis',(-0.707106781186548,0.,0.707106781186547));
#4133=DIRECTION('ref_axis',(-0.707106781186547,0.,-0.707106781186548));
#4134=DIRECTION('center_axis',(0.707106781186548,0.,-0.707106781186547));
#4135=DIRECTION('ref_axis',(-0.707106781186547,0.,-0.707106781186548));
#4136=DIRECTION('center_axis',(0.707106781186548,0.,-0.707106781186547));
#4137=DIRECTION('ref_axis',(-0.707106781186547,0.,-0.707106781186548));
#4138=DIRECTION('',(-0.707106781186548,0.,0.707106781186547));
#4139=DIRECTION('center_axis',(0.707106781186548,0.,-0.707106781186547));
#4140=DIRECTION('ref_axis',(-0.707106781186547,0.,-0.707106781186548));
#4141=DIRECTION('center_axis',(0.707106781186548,0.,-0.707106781186547));
#4142=DIRECTION('ref_axis',(-0.707106781186547,0.,-0.707106781186548));
#4143=DIRECTION('center_axis',(0.707106781186548,0.,-0.707106781186547));
#4144=DIRECTION('ref_axis',(-0.707106781186547,0.,-0.707106781186548));
#4145=DIRECTION('axis',(0.,0.,1.));
#4146=DIRECTION('refdir',(1.,0.,0.));
#4147=DIRECTION('center_axis',(0.707106781186548,0.,-0.707106781186547));
#4148=DIRECTION('ref_axis',(-0.707106781186547,0.,-0.707106781186548));
#4149=DIRECTION('center_axis',(-0.707106781186548,0.,0.707106781186547));
#4150=DIRECTION('ref_axis',(-0.707106781186547,0.,-0.707106781186548));
#4151=DIRECTION('',(-0.707106781186548,0.,0.707106781186547));
#4152=DIRECTION('center_axis',(-0.707106781186548,0.,0.707106781186547));
#4153=DIRECTION('ref_axis',(-0.707106781186547,0.,-0.707106781186548));
#4154=DIRECTION('center_axis',(0.707106781186548,0.,-0.707106781186547));
#4155=DIRECTION('ref_axis',(-0.707106781186547,0.,-0.707106781186548));
#4156=DIRECTION('center_axis',(0.707106781186548,0.,-0.707106781186547));
#4157=DIRECTION('ref_axis',(-0.707106781186547,0.,-0.707106781186548));
#4158=DIRECTION('',(-0.707106781186548,0.,0.707106781186547));
#4159=DIRECTION('center_axis',(0.707106781186548,0.,-0.707106781186547));
#4160=DIRECTION('ref_axis',(-0.707106781186547,0.,-0.707106781186548));
#4161=DIRECTION('center_axis',(0.707106781186548,0.,-0.707106781186547));
#4162=DIRECTION('ref_axis',(-0.707106781186547,0.,-0.707106781186548));
#4163=DIRECTION('center_axis',(0.707106781186548,0.,-0.707106781186547));
#4164=DIRECTION('ref_axis',(-0.707106781186547,0.,-0.707106781186548));
#4165=DIRECTION('axis',(0.,0.,1.));
#4166=DIRECTION('refdir',(1.,0.,0.));
#4167=DIRECTION('center_axis',(0.707106781186548,0.,-0.707106781186547));
#4168=DIRECTION('ref_axis',(-0.707106781186547,0.,-0.707106781186548));
#4169=DIRECTION('center_axis',(0.707106781186548,0.,-0.707106781186547));
#4170=DIRECTION('ref_axis',(-0.707106781186547,0.,-0.707106781186548));
#4171=DIRECTION('',(0.707106781186548,0.,-0.707106781186547));
#4172=DIRECTION('center_axis',(-0.707106781186548,0.,0.707106781186547));
#4173=DIRECTION('ref_axis',(-0.707106781186547,0.,-0.707106781186548));
#4174=DIRECTION('center_axis',(0.707106781186548,0.,-0.707106781186547));
#4175=DIRECTION('ref_axis',(-0.707106781186547,0.,-0.707106781186548));
#4176=DIRECTION('center_axis',(0.707106781186548,0.,-0.707106781186547));
#4177=DIRECTION('ref_axis',(-0.707106781186547,0.,-0.707106781186548));
#4178=DIRECTION('',(0.707106781186548,0.,-0.707106781186547));
#4179=DIRECTION('center_axis',(-0.707106781186548,0.,0.707106781186547));
#4180=DIRECTION('ref_axis',(-0.707106781186547,0.,-0.707106781186548));
#4181=DIRECTION('center_axis',(0.707106781186548,0.,-0.707106781186547));
#4182=DIRECTION('ref_axis',(-0.707106781186547,0.,-0.707106781186548));
#4183=DIRECTION('center_axis',(0.707106781186548,0.,-0.707106781186547));
#4184=DIRECTION('ref_axis',(-0.707106781186547,0.,-0.707106781186548));
#4185=DIRECTION('',(0.707106781186548,0.,-0.707106781186547));
#4186=DIRECTION('center_axis',(-0.707106781186548,0.,0.707106781186547));
#4187=DIRECTION('ref_axis',(-0.707106781186547,0.,-0.707106781186548));
#4188=DIRECTION('center_axis',(0.707106781186548,0.,-0.707106781186547));
#4189=DIRECTION('ref_axis',(-0.707106781186547,0.,-0.707106781186548));
#4190=DIRECTION('center_axis',(0.707106781186548,0.,-0.707106781186547));
#4191=DIRECTION('ref_axis',(-0.707106781186547,0.,-0.707106781186548));
#4192=DIRECTION('',(0.707106781186548,0.,-0.707106781186547));
#4193=DIRECTION('center_axis',(-0.707106781186548,0.,0.707106781186547));
#4194=DIRECTION('ref_axis',(-0.707106781186547,0.,-0.707106781186548));
#4195=DIRECTION('center_axis',(0.707106781186548,0.,-0.707106781186547));
#4196=DIRECTION('ref_axis',(-0.707106781186547,0.,-0.707106781186548));
#4197=DIRECTION('center_axis',(-0.707106781186548,0.,0.707106781186547));
#4198=DIRECTION('ref_axis',(-0.707106781186547,0.,-0.707106781186548));
#4199=DIRECTION('',(-0.707106781186548,0.,0.707106781186547));
#4200=DIRECTION('center_axis',(-0.707106781186548,0.,0.707106781186547));
#4201=DIRECTION('ref_axis',(-0.707106781186547,0.,-0.707106781186548));
#4202=DIRECTION('center_axis',(0.707106781186548,0.,-0.707106781186547));
#4203=DIRECTION('ref_axis',(-0.707106781186547,0.,-0.707106781186548));
#4204=DIRECTION('center_axis',(0.707106781186548,0.,-0.707106781186547));
#4205=DIRECTION('ref_axis',(-0.707106781186547,0.,-0.707106781186548));
#4206=DIRECTION('',(-0.707106781186548,0.,0.707106781186547));
#4207=DIRECTION('center_axis',(0.707106781186548,0.,-0.707106781186547));
#4208=DIRECTION('ref_axis',(-0.707106781186547,0.,-0.707106781186548));
#4209=DIRECTION('center_axis',(0.707106781186548,0.,-0.707106781186547));
#4210=DIRECTION('ref_axis',(-0.707106781186547,0.,-0.707106781186548));
#4211=DIRECTION('center_axis',(0.707106781186548,0.,-0.707106781186547));
#4212=DIRECTION('ref_axis',(-0.707106781186547,0.,-0.707106781186548));
#4213=DIRECTION('axis',(0.,0.,1.));
#4214=DIRECTION('refdir',(1.,0.,0.));
#4215=DIRECTION('center_axis',(0.707106781186548,0.,-0.707106781186547));
#4216=DIRECTION('ref_axis',(-0.707106781186547,0.,-0.707106781186548));
#4217=DIRECTION('center_axis',(0.707106781186548,0.,-0.707106781186547));
#4218=DIRECTION('ref_axis',(-0.707106781186547,0.,-0.707106781186548));
#4219=DIRECTION('',(0.707106781186548,0.,-0.707106781186547));
#4220=DIRECTION('center_axis',(-0.707106781186548,0.,0.707106781186547));
#4221=DIRECTION('ref_axis',(-0.707106781186547,0.,-0.707106781186548));
#4222=DIRECTION('center_axis',(0.707106781186548,0.,-0.707106781186547));
#4223=DIRECTION('ref_axis',(-0.707106781186547,0.,-0.707106781186548));
#4224=DIRECTION('center_axis',(0.707106781186548,0.,-0.707106781186547));
#4225=DIRECTION('ref_axis',(-0.707106781186547,0.,-0.707106781186548));
#4226=DIRECTION('',(0.707106781186548,0.,-0.707106781186547));
#4227=DIRECTION('center_axis',(-0.707106781186548,0.,0.707106781186547));
#4228=DIRECTION('ref_axis',(-0.707106781186547,0.,-0.707106781186548));
#4229=DIRECTION('center_axis',(0.707106781186548,0.,-0.707106781186547));
#4230=DIRECTION('ref_axis',(-0.707106781186547,0.,-0.707106781186548));
#4231=DIRECTION('center_axis',(0.707106781186548,0.,-0.707106781186547));
#4232=DIRECTION('ref_axis',(-0.707106781186547,0.,-0.707106781186548));
#4233=DIRECTION('',(0.707106781186548,0.,-0.707106781186547));
#4234=DIRECTION('center_axis',(-0.707106781186548,0.,0.707106781186547));
#4235=DIRECTION('ref_axis',(-0.707106781186547,0.,-0.707106781186548));
#4236=DIRECTION('center_axis',(0.707106781186548,0.,-0.707106781186547));
#4237=DIRECTION('ref_axis',(-0.707106781186547,0.,-0.707106781186548));
#4238=DIRECTION('center_axis',(0.707106781186548,0.,-0.707106781186547));
#4239=DIRECTION('ref_axis',(-0.707106781186547,0.,-0.707106781186548));
#4240=DIRECTION('',(0.707106781186548,0.,-0.707106781186547));
#4241=DIRECTION('center_axis',(-0.707106781186548,0.,0.707106781186547));
#4242=DIRECTION('ref_axis',(-0.707106781186547,0.,-0.707106781186548));
#4243=DIRECTION('center_axis',(0.707106781186548,0.,-0.707106781186547));
#4244=DIRECTION('ref_axis',(-0.707106781186547,0.,-0.707106781186548));
#4245=DIRECTION('center_axis',(0.707106781186548,0.,-0.707106781186547));
#4246=DIRECTION('ref_axis',(-0.707106781186547,0.,-0.707106781186548));
#4247=DIRECTION('',(0.707106781186548,0.,-0.707106781186547));
#4248=DIRECTION('center_axis',(-0.707106781186548,0.,0.707106781186547));
#4249=DIRECTION('ref_axis',(-0.707106781186547,0.,-0.707106781186548));
#4250=DIRECTION('center_axis',(0.707106781186548,0.,-0.707106781186547));
#4251=DIRECTION('ref_axis',(-0.707106781186547,0.,-0.707106781186548));
#4252=DIRECTION('center_axis',(0.707106781186548,0.,-0.707106781186547));
#4253=DIRECTION('ref_axis',(-0.707106781186547,0.,-0.707106781186548));
#4254=DIRECTION('',(-0.707106781186548,0.,0.707106781186547));
#4255=DIRECTION('center_axis',(0.707106781186548,0.,-0.707106781186547));
#4256=DIRECTION('ref_axis',(-0.707106781186547,0.,-0.707106781186548));
#4257=DIRECTION('center_axis',(0.707106781186548,0.,-0.707106781186547));
#4258=DIRECTION('ref_axis',(-0.707106781186547,0.,-0.707106781186548));
#4259=DIRECTION('center_axis',(0.707106781186548,0.,-0.707106781186547));
#4260=DIRECTION('ref_axis',(-0.707106781186547,0.,-0.707106781186548));
#4261=DIRECTION('center_axis',(0.707106781186548,0.,-0.707106781186547));
#4262=DIRECTION('ref_axis',(-0.707106781186547,0.,-0.707106781186548));
#4263=DIRECTION('',(-0.707106781186548,0.,0.707106781186547));
#4264=DIRECTION('center_axis',(0.707106781186548,0.,-0.707106781186547));
#4265=DIRECTION('ref_axis',(-0.707106781186547,0.,-0.707106781186548));
#4266=DIRECTION('center_axis',(0.707106781186548,0.,-0.707106781186547));
#4267=DIRECTION('ref_axis',(-0.707106781186547,0.,-0.707106781186548));
#4268=DIRECTION('center_axis',(0.707106781186548,0.,-0.707106781186547));
#4269=DIRECTION('ref_axis',(-0.707106781186547,0.,-0.707106781186548));
#4270=DIRECTION('axis',(0.,0.,1.));
#4271=DIRECTION('refdir',(1.,0.,0.));
#4272=DIRECTION('center_axis',(0.,1.,0.));
#4273=DIRECTION('ref_axis',(0.,0.,1.));
#4274=DIRECTION('center_axis',(0.,-1.,0.));
#4275=DIRECTION('ref_axis',(1.,0.,0.));
#4276=DIRECTION('center_axis',(0.,-1.,0.));
#4277=DIRECTION('ref_axis',(1.,0.,0.));
#4278=DIRECTION('center_axis',(0.,-1.,0.));
#4279=DIRECTION('ref_axis',(1.,0.,0.));
#4280=DIRECTION('',(0.707106781186548,0.707106781186547,8.65956056235494E-17));
#4281=DIRECTION('center_axis',(0.,-1.,0.));
#4282=DIRECTION('ref_axis',(1.,0.,0.));
#4283=DIRECTION('center_axis',(0.,-1.,0.));
#4284=DIRECTION('ref_axis',(1.,0.,0.));
#4285=DIRECTION('',(0.,1.,0.));
#4286=DIRECTION('center_axis',(0.,1.,0.));
#4287=DIRECTION('ref_axis',(1.,0.,0.));
#4288=DIRECTION('center_axis',(0.,-1.,0.));
#4289=DIRECTION('ref_axis',(1.,0.,0.));
#4290=DIRECTION('',(-0.707106781186547,0.707106781186548,-8.65956056235493E-17));
#4291=DIRECTION('center_axis',(0.,-1.,0.));
#4292=DIRECTION('ref_axis',(0.,0.,-1.));
#4293=DIRECTION('center_axis',(0.,-1.,0.));
#4294=DIRECTION('ref_axis',(1.,0.,0.));
#4295=DIRECTION('center_axis',(0.,1.,0.));
#4296=DIRECTION('ref_axis',(1.,0.,0.));
#4297=DIRECTION('center_axis',(0.,1.,0.));
#4298=DIRECTION('ref_axis',(1.,0.,0.));
#4299=DIRECTION('',(-0.447213595499958,0.894427190999916,-5.47678698264203E-17));
#4300=DIRECTION('center_axis',(0.,-1.,0.));
#4301=DIRECTION('ref_axis',(1.,0.,0.));
#4302=DIRECTION('center_axis',(0.,1.,0.));
#4303=DIRECTION('ref_axis',(1.,0.,0.));
#4304=DIRECTION('',(0.,1.,0.));
#4305=DIRECTION('center_axis',(0.,1.,0.));
#4306=DIRECTION('ref_axis',(1.,0.,0.));
#4307=DIRECTION('center_axis',(0.,-1.,0.));
#4308=DIRECTION('ref_axis',(1.,0.,0.));
#4309=DIRECTION('',(-0.707106781186547,0.707106781186548,-8.65956056235493E-17));
#4310=DIRECTION('center_axis',(0.,-1.,0.));
#4311=DIRECTION('ref_axis',(0.,0.,-1.));
#4312=DIRECTION('center_axis',(0.866025403784439,0.,-0.5));
#4313=DIRECTION('ref_axis',(0.5,0.,0.866025403784439));
#4314=DIRECTION('',(-0.5,0.,-0.866025403784439));
#4315=DIRECTION('',(0.,-1.,0.));
#4316=DIRECTION('',(0.5,0.,0.866025403784439));
#4317=DIRECTION('',(0.,-1.,0.));
#4318=DIRECTION('center_axis',(1.92296268638356E-16,0.,-1.));
#4319=DIRECTION('ref_axis',(1.,0.,1.92296268638356E-16));
#4320=DIRECTION('',(-1.,0.,-1.92296268638356E-16));
#4321=DIRECTION('',(0.,-1.,0.));
#4322=DIRECTION('',(1.,0.,1.92296268638356E-16));
#4323=DIRECTION('center_axis',(-0.866025403784439,0.,-0.5));
#4324=DIRECTION('ref_axis',(0.5,0.,-0.866025403784439));
#4325=DIRECTION('',(-0.5,0.,0.866025403784438));
#4326=DIRECTION('',(0.,-1.,0.));
#4327=DIRECTION('',(0.5,0.,-0.866025403784438));
#4328=DIRECTION('center_axis',(-0.866025403784439,0.,0.5));
#4329=DIRECTION('ref_axis',(-0.5,0.,-0.866025403784439));
#4330=DIRECTION('',(0.5,0.,0.866025403784439));
#4331=DIRECTION('',(0.,-1.,0.));
#4332=DIRECTION('',(-0.5,0.,-0.866025403784439));
#4333=DIRECTION('center_axis',(-1.92296268638356E-16,0.,1.));
#4334=DIRECTION('ref_axis',(-1.,0.,-1.92296268638356E-16));
#4335=DIRECTION('',(1.,0.,1.92296268638356E-16));
#4336=DIRECTION('',(0.,-1.,0.));
#4337=DIRECTION('',(-1.,0.,-1.92296268638356E-16));
#4338=DIRECTION('center_axis',(0.866025403784439,0.,0.5));
#4339=DIRECTION('ref_axis',(-0.5,0.,0.866025403784439));
#4340=DIRECTION('',(0.5,0.,-0.866025403784439));
#4341=DIRECTION('',(-0.5,0.,0.866025403784439));
#4342=DIRECTION('center_axis',(0.,1.,0.));
#4343=DIRECTION('ref_axis',(1.,0.,0.));
#4344=DIRECTION('center_axis',(0.,-1.,0.));
#4345=DIRECTION('ref_axis',(0.,0.,-1.));
#4346=DIRECTION('axis',(0.,0.,1.));
#4347=DIRECTION('refdir',(1.,0.,0.));
#4348=DIRECTION('center_axis',(0.,1.,0.));
#4349=DIRECTION('ref_axis',(1.,0.,0.));
#4350=DIRECTION('',(-0.5,0.,0.866025403784439));
#4351=DIRECTION('',(-1.,0.,-2.84883360945713E-16));
#4352=DIRECTION('',(-0.5,0.,-0.866025403784439));
#4353=DIRECTION('',(0.5,0.,-0.866025403784439));
#4354=DIRECTION('',(1.,0.,0.));
#4355=DIRECTION('',(0.5,0.,0.866025403784439));
#4356=DIRECTION('center_axis',(0.,-1.,0.));
#4357=DIRECTION('ref_axis',(1.,0.,0.));
#4358=DIRECTION('center_axis',(0.,1.,0.));
#4359=DIRECTION('ref_axis',(1.,0.,0.));
#4360=DIRECTION('',(0.5,0.,-0.866025403784439));
#4361=DIRECTION('',(-0.5,0.,-0.866025403784439));
#4362=DIRECTION('',(-1.,0.,0.));
#4363=DIRECTION('',(-0.5,0.,0.866025403784439));
#4364=DIRECTION('',(0.5,0.,0.866025403784439));
#4365=DIRECTION('',(1.,0.,2.84883360945713E-16));
#4366=DIRECTION('center_axis',(0.,1.,0.));
#4367=DIRECTION('ref_axis',(1.,0.,0.));
#4368=DIRECTION('center_axis',(-2.84883360945713E-16,0.,1.));
#4369=DIRECTION('ref_axis',(1.,0.,2.84883360945713E-16));
#4370=DIRECTION('',(0.,-1.,0.));
#4371=DIRECTION('',(0.,1.,0.));
#4372=DIRECTION('center_axis',(-0.866025403784439,0.,0.5));
#4373=DIRECTION('ref_axis',(0.5,0.,0.866025403784439));
#4374=DIRECTION('',(0.,1.,0.));
#4375=DIRECTION('center_axis',(-0.866025403784439,0.,-0.5));
#4376=DIRECTION('ref_axis',(-0.5,0.,0.866025403784439));
#4377=DIRECTION('',(0.,1.,0.));
#4378=DIRECTION('center_axis',(0.,0.,-1.));
#4379=DIRECTION('ref_axis',(-1.,0.,0.));
#4380=DIRECTION('',(0.,1.,0.));
#4381=DIRECTION('center_axis',(0.866025403784439,0.,-0.5));
#4382=DIRECTION('ref_axis',(-0.5,0.,-0.866025403784439));
#4383=DIRECTION('',(0.,1.,0.));
#4384=DIRECTION('center_axis',(0.866025403784439,0.,0.5));
#4385=DIRECTION('ref_axis',(0.5,0.,-0.866025403784439));
#4386=DIRECTION('center_axis',(0.,-1.,0.));
#4387=DIRECTION('ref_axis',(1.,0.,0.));
#4388=DIRECTION('',(0.,1.,0.));
#4389=DIRECTION('center_axis',(0.,-1.,0.));
#4390=DIRECTION('ref_axis',(1.,0.,0.));
#4391=DIRECTION('center_axis',(0.,1.,0.));
#4392=DIRECTION('ref_axis',(0.,0.,1.));
#4393=DIRECTION('center_axis',(0.,-1.,0.));
#4394=DIRECTION('ref_axis',(1.,0.,0.));
#4395=DIRECTION('center_axis',(0.,-1.,0.));
#4396=DIRECTION('ref_axis',(1.,0.,0.));
#4397=DIRECTION('center_axis',(0.,-1.,0.));
#4398=DIRECTION('ref_axis',(1.,0.,0.));
#4399=DIRECTION('',(0.707106781186547,0.707106781186548,8.65956056235493E-17));
#4400=DIRECTION('center_axis',(0.,-1.,0.));
#4401=DIRECTION('ref_axis',(1.,0.,0.));
#4402=DIRECTION('center_axis',(0.,-1.,0.));
#4403=DIRECTION('ref_axis',(1.,0.,0.));
#4404=DIRECTION('',(0.,1.,0.));
#4405=DIRECTION('center_axis',(0.,1.,0.));
#4406=DIRECTION('ref_axis',(1.,0.,0.));
#4407=DIRECTION('center_axis',(0.,-1.,0.));
#4408=DIRECTION('ref_axis',(1.,0.,0.));
#4409=DIRECTION('',(-0.707106781186547,0.707106781186548,-8.65956056235493E-17));
#4410=DIRECTION('center_axis',(0.,-1.,0.));
#4411=DIRECTION('ref_axis',(0.,0.,-1.));
#4412=DIRECTION('center_axis',(0.,-1.,0.));
#4413=DIRECTION('ref_axis',(1.,0.,0.));
#4414=DIRECTION('center_axis',(0.,-1.,0.));
#4415=DIRECTION('ref_axis',(1.,0.,0.));
#4416=DIRECTION('',(0.,1.,0.));
#4417=DIRECTION('axis',(0.,0.,1.));
#4418=DIRECTION('refdir',(1.,0.,0.));
#4419=DIRECTION('center_axis',(1.,0.,0.));
#4420=DIRECTION('ref_axis',(0.,0.,-1.));
#4421=DIRECTION('',(0.,0.5,0.866025403784439));
#4422=DIRECTION('',(0.,1.,-4.39534328316243E-16));
#4423=DIRECTION('',(0.,0.5,-0.866025403784439));
#4424=DIRECTION('',(0.,-0.5,-0.866025403784439));
#4425=DIRECTION('',(0.,-1.,0.));
#4426=DIRECTION('',(0.,-0.5,0.866025403784439));
#4427=DIRECTION('center_axis',(1.,0.,0.));
#4428=DIRECTION('ref_axis',(0.,0.,-1.));
#4429=DIRECTION('center_axis',(0.,-4.39534328316243E-16,-1.));
#4430=DIRECTION('ref_axis',(0.,1.,-4.39534328316243E-16));
#4431=DIRECTION('',(1.,0.,0.));
#4432=DIRECTION('',(0.,1.,-4.39534328316243E-16));
#4433=DIRECTION('',(1.,0.,0.));
#4434=DIRECTION('center_axis',(0.,-0.866025403784439,-0.5));
#4435=DIRECTION('ref_axis',(0.,0.5,-0.866025403784439));
#4436=DIRECTION('',(0.,0.5,-0.866025403784439));
#4437=DIRECTION('',(1.,0.,0.));
#4438=DIRECTION('center_axis',(0.,-0.866025403784439,0.5));
#4439=DIRECTION('ref_axis',(0.,-0.5,-0.866025403784439));
#4440=DIRECTION('',(0.,-0.5,-0.866025403784439));
#4441=DIRECTION('',(1.,0.,0.));
#4442=DIRECTION('center_axis',(0.,0.,1.));
#4443=DIRECTION('ref_axis',(0.,-1.,0.));
#4444=DIRECTION('',(0.,-1.,0.));
#4445=DIRECTION('',(1.,0.,0.));
#4446=DIRECTION('center_axis',(0.,0.866025403784439,0.5));
#4447=DIRECTION('ref_axis',(0.,-0.5,0.866025403784439));
#4448=DIRECTION('',(0.,-0.5,0.866025403784439));
#4449=DIRECTION('',(1.,0.,0.));
#4450=DIRECTION('center_axis',(0.,0.866025403784439,-0.5));
#4451=DIRECTION('ref_axis',(0.,0.5,0.866025403784439));
#4452=DIRECTION('',(0.,0.5,0.866025403784439));
#4453=DIRECTION('center_axis',(1.,0.,0.));
#4454=DIRECTION('ref_axis',(0.,0.,-1.));
#4455=DIRECTION('center_axis',(1.,0.,0.));
#4456=DIRECTION('ref_axis',(0.,0.,-1.));
#4457=DIRECTION('',(-1.,0.,0.));
#4458=DIRECTION('center_axis',(1.,0.,0.));
#4459=DIRECTION('ref_axis',(0.,0.,-1.));
#4460=DIRECTION('center_axis',(1.,0.,0.));
#4461=DIRECTION('ref_axis',(0.,0.,-1.));
#4462=DIRECTION('',(0.,0.,1.));
#4463=DIRECTION('',(1.,0.,0.));
#4464=DIRECTION('',(0.,0.,1.));
#4465=DIRECTION('',(1.,0.,0.));
#4466=DIRECTION('',(0.,0.,1.));
#4467=DIRECTION('',(1.,0.,0.));
#4468=DIRECTION('',(0.,0.,1.));
#4469=DIRECTION('',(1.,0.,0.));
#4470=DIRECTION('',(0.,0.,1.));
#4471=DIRECTION('',(1.,0.,0.));
#4472=DIRECTION('',(0.,0.,1.));
#4473=DIRECTION('',(1.,0.,0.));
#4474=DIRECTION('',(1.57009245868378E-16,-1.,-1.57009245868377E-16));
#4475=DIRECTION('',(-0.707106781186547,0.,-0.707106781186548));
#4476=DIRECTION('',(1.57009245868378E-16,-1.,-1.57009245868377E-16));
#4477=DIRECTION('',(-0.707106781186547,0.,-0.707106781186548));
#4478=DIRECTION('',(1.57009245868378E-16,-1.,-1.57009245868377E-16));
#4479=DIRECTION('',(-0.707106781186547,0.,-0.707106781186548));
#4480=DIRECTION('',(1.57009245868378E-16,-1.,-1.57009245868377E-16));
#4481=DIRECTION('',(-0.707106781186547,0.,-0.707106781186548));
#4482=DIRECTION('',(0.,0.,1.));
#4483=DIRECTION('',(2.22044604925031E-16,-1.,0.));
#4484=DIRECTION('',(0.,0.,1.));
#4485=DIRECTION('',(2.22044604925031E-16,-1.,0.));
#4486=DIRECTION('',(0.707106781186548,0.,0.707106781186547));
#4487=DIRECTION('',(0.707106781186547,0.,-0.707106781186548));
#4488=DIRECTION('',(0.,0.,1.));
#4489=DIRECTION('',(1.,0.,0.));
#4490=CARTESIAN_POINT('',(0.,0.,0.));
#4491=CARTESIAN_POINT('',(0.,0.,0.));
#4492=CARTESIAN_POINT('',(0.,0.,0.));
#4493=CARTESIAN_POINT('Origin',(2.11335136523794,-1.69705627484771,1.48664863476206));
#4494=CARTESIAN_POINT('',(2.36083873865323,-1.69705627484771,1.59271465194004));
#4495=CARTESIAN_POINT('Origin',(2.1840620433566,-1.69705627484771,1.41593795664341));
#4496=CARTESIAN_POINT('',(2.92652416360247,-1.69705627484771,1.0270292269908));
#4497=CARTESIAN_POINT('',(2.29012806053458,-1.69705627484771,1.6634253300587));
#4498=CARTESIAN_POINT('Origin',(2.74974746830583,-1.69705627484771,0.850252531694168));
#4499=CARTESIAN_POINT('Origin',(2.11335136523794,1.69705627484771,1.48664863476206));
#4500=CARTESIAN_POINT('',(2.36083873865323,1.69705627484771,1.59271465194004));
#4501=CARTESIAN_POINT('Origin',(2.1840620433566,1.69705627484771,1.41593795664341));
#4502=CARTESIAN_POINT('',(2.92652416360247,1.69705627484771,1.0270292269908));
#4503=CARTESIAN_POINT('',(2.29012806053458,1.69705627484771,1.6634253300587));
#4504=CARTESIAN_POINT('Origin',(2.74974746830583,1.69705627484771,0.850252531694167));
#4505=CARTESIAN_POINT('Origin',(4.51335136523794,1.69705627484771,3.88664863476206));
#4506=CARTESIAN_POINT('',(4.76083873865323,1.69705627484771,3.99271465194004));
#4507=CARTESIAN_POINT('Origin',(4.5840620433566,1.69705627484771,3.81593795664341));
#4508=CARTESIAN_POINT('',(5.32652416360247,1.69705627484771,3.42702922699081));
#4509=CARTESIAN_POINT('',(4.69012806053458,1.69705627484771,4.0634253300587));
#4510=CARTESIAN_POINT('Origin',(5.14974746830583,1.69705627484771,3.25025253169417));
#4511=CARTESIAN_POINT('Origin',(4.51335136523794,-1.69705627484771,3.88664863476206));
#4512=CARTESIAN_POINT('',(4.76083873865323,-1.69705627484771,3.99271465194004));
#4513=CARTESIAN_POINT('Origin',(4.5840620433566,-1.69705627484771,3.81593795664341));
#4514=CARTESIAN_POINT('',(5.32652416360247,-1.69705627484771,3.42702922699081));
#4515=CARTESIAN_POINT('',(4.69012806053458,-1.69705627484771,4.0634253300587));
#4516=CARTESIAN_POINT('Origin',(5.14974746830583,-1.69705627484771,3.25025253169417));
#4517=CARTESIAN_POINT('Origin',(-0.575735931288071,0.,6.57573593128807));
#4518=CARTESIAN_POINT('',(0.515222755900927,-0.42381397534026,7.66669461847707));
#4519=CARTESIAN_POINT('',(0.5,-0.446860618394116,7.65147186257614));
#4520=CARTESIAN_POINT('Origin',(-0.151471862576143,0.,7.));
#4521=CARTESIAN_POINT('',(0.515222755900927,0.42381397534026,7.66669461847707));
#4522=CARTESIAN_POINT('Origin',(-0.575735931288071,0.,6.57573593128807));
#4523=CARTESIAN_POINT('',(0.5,0.446860618394116,7.65147186257614));
#4524=CARTESIAN_POINT('Origin',(-0.151471862576143,0.,7.));
#4525=CARTESIAN_POINT('',(0.5,0.,7.65147186257614));
#4526=CARTESIAN_POINT('',(0.138441917710342,-1.23689326713883E-16,7.28991378028648));
#4527=CARTESIAN_POINT('Origin',(-0.575735931288071,0.,6.57573593128807));
#4528=CARTESIAN_POINT('Origin',(-0.575735931288071,0.,6.57573593128807));
#4529=CARTESIAN_POINT('',(2.05274169979695,-7.76612318099432E-18,6.21));
#4530=CARTESIAN_POINT('Ctrl Pts',(0.515222755900927,0.423813975340259,7.66669461847707));
#4531=CARTESIAN_POINT('Ctrl Pts',(0.526116666884646,0.467880373133453,7.63868186014655));
#4532=CARTESIAN_POINT('Ctrl Pts',(0.53939367180672,0.508081707628242,7.60688542097163));
#4533=CARTESIAN_POINT('Ctrl Pts',(0.573486312745389,0.586129881875093,7.53294329022174));
#4534=CARTESIAN_POINT('Ctrl Pts',(0.596451435323986,0.624301170571409,7.48753051107401));
#4535=CARTESIAN_POINT('Ctrl Pts',(0.65156518194746,0.68858835699378,7.39151504429253));
#4536=CARTESIAN_POINT('Ctrl Pts',(0.683747388356032,0.714719578864005,7.34094189934536));
#4537=CARTESIAN_POINT('Ctrl Pts',(0.791807275601753,0.774755581890673,7.18899251283438));
#4538=CARTESIAN_POINT('Ctrl Pts',(0.88020875365155,0.79,7.08748024616524));
#4539=CARTESIAN_POINT('Ctrl Pts',(1.08628177383383,0.79,6.88140722598296));
#4540=CARTESIAN_POINT('Ctrl Pts',(1.22448970987637,0.76321488961253,6.76575702265008));
#4541=CARTESIAN_POINT('Ctrl Pts',(1.5022165321408,0.66455929680406,6.55758880230742));
#4542=CARTESIAN_POINT('Ctrl Pts',(1.64147614223073,0.592948544581024,6.46460220651928));
#4543=CARTESIAN_POINT('Ctrl Pts',(1.83272612115297,0.444293338230863,6.34266823160953));
#4544=CARTESIAN_POINT('Ctrl Pts',(1.90715208192005,0.371863087636435,6.29702949928263));
#4545=CARTESIAN_POINT('Ctrl Pts',(1.98979747291659,0.244143424893146,6.24728394566456));
#4546=CARTESIAN_POINT('Ctrl Pts',(2.01256955325863,0.198394270739821,6.23374920803759));
#4547=CARTESIAN_POINT('Ctrl Pts',(2.04404821289531,0.102192836977527,6.21510689448735));
#4548=CARTESIAN_POINT('Ctrl Pts',(2.05274169979695,0.0517361417724,6.21));
#4549=CARTESIAN_POINT('Ctrl Pts',(2.05274169979695,2.63677968348475E-16,
6.21));
#4550=CARTESIAN_POINT('Ctrl Pts',(2.05274169979695,1.80411241501588E-16,
6.21));
#4551=CARTESIAN_POINT('Ctrl Pts',(2.05274169979695,-0.0517361417723996,
6.21));
#4552=CARTESIAN_POINT('Ctrl Pts',(2.04404821289531,-0.102192836977527,6.21510689448735));
#4553=CARTESIAN_POINT('Ctrl Pts',(2.01256955325863,-0.19839427073982,6.23374920803759));
#4554=CARTESIAN_POINT('Ctrl Pts',(1.98979747291659,-0.244143424893145,6.24728394566456));
#4555=CARTESIAN_POINT('Ctrl Pts',(1.90715208192005,-0.371863087636433,6.29702949928263));
#4556=CARTESIAN_POINT('Ctrl Pts',(1.83272612115297,-0.444293338230862,6.34266823160953));
#4557=CARTESIAN_POINT('Ctrl Pts',(1.64147614223073,-0.592948544581024,6.46460220651928));
#4558=CARTESIAN_POINT('Ctrl Pts',(1.5022165321408,-0.66455929680406,6.55758880230742));
#4559=CARTESIAN_POINT('Ctrl Pts',(1.22448970987637,-0.763214889612529,6.76575702265008));
#4560=CARTESIAN_POINT('Ctrl Pts',(1.08628177383383,-0.79,6.88140722598296));
#4561=CARTESIAN_POINT('Ctrl Pts',(0.96768899981679,-0.79,7.));
#4562=CARTESIAN_POINT('Ctrl Pts',(0.88020875365155,-0.79,7.08748024616524));
#4563=CARTESIAN_POINT('Ctrl Pts',(0.791807275601753,-0.774755581890674,
7.18899251283438));
#4564=CARTESIAN_POINT('Ctrl Pts',(0.683747388356032,-0.714719578864005,
7.34094189934535));
#4565=CARTESIAN_POINT('Ctrl Pts',(0.651565181947462,-0.68858835699378,7.39151504429253));
#4566=CARTESIAN_POINT('Ctrl Pts',(0.596451435323987,-0.624301170571409,
7.487530511074));
#4567=CARTESIAN_POINT('Ctrl Pts',(0.573486312745389,-0.586129881875093,
7.53294329022174));
#4568=CARTESIAN_POINT('Ctrl Pts',(0.539393671847301,-0.508081707721144,
7.60688542088362));
#4569=CARTESIAN_POINT('Ctrl Pts',(0.526116666881167,-0.467880373119377,
7.63868186015549));
#4570=CARTESIAN_POINT('Ctrl Pts',(0.515222755900927,-0.423813975340259,
7.66669461847707));
#4571=CARTESIAN_POINT('',(5.08111831820431,1.95943487863577E-16,3.18162338159264));
#4572=CARTESIAN_POINT('',(0.555634918610405,-1.95943487863577E-16,7.70710678118655));
#4573=CARTESIAN_POINT('Origin',(3.94974746830583,0.,2.05025253169417));
#4574=CARTESIAN_POINT('Origin',(0.5,0.,7.));
#4575=CARTESIAN_POINT('',(0.5,-9.67470971326409E-17,7.79));
#4576=CARTESIAN_POINT('Origin',(0.5,0.,7.));
#4577=CARTESIAN_POINT('Origin',(0.5,0.,7.));
#4578=CARTESIAN_POINT('Origin',(-1.,0.,7.));
#4579=CARTESIAN_POINT('',(-1.62928530890209,-0.477598157450382,6.37071469109791));
#4580=CARTESIAN_POINT('',(-1.62928530890209,0.477598157450382,6.37071469109791));
#4581=CARTESIAN_POINT('Ctrl Pts',(-1.62928530890209,-0.477598157450382,
6.37071469109791));
#4582=CARTESIAN_POINT('Ctrl Pts',(-1.62928530890209,-0.425917629345584,
6.33149158410694));
#4583=CARTESIAN_POINT('Ctrl Pts',(-1.63106209224364,-0.368165804555039,
6.29790350040073));
#4584=CARTESIAN_POINT('Ctrl Pts',(-1.63576347459867,-0.208570757814752,
6.23055387445547));
#4585=CARTESIAN_POINT('Ctrl Pts',(-1.63835569799683,-0.101035232793328,
6.21));
#4586=CARTESIAN_POINT('Ctrl Pts',(-1.63835569799683,0.101035232793328,6.21));
#4587=CARTESIAN_POINT('Ctrl Pts',(-1.63576347459867,0.208570757814752,6.23055387445547));
#4588=CARTESIAN_POINT('Ctrl Pts',(-1.63106209224364,0.368165804555039,6.29790350040073));
#4589=CARTESIAN_POINT('Ctrl Pts',(-1.62928530890209,0.425917629345584,6.33149158410694));
#4590=CARTESIAN_POINT('Ctrl Pts',(-1.62928530890209,0.477598157450382,6.37071469109791));
#4591=CARTESIAN_POINT('',(-0.285822151001587,-1.23689326713883E-16,7.71417784899841));
#4592=CARTESIAN_POINT('Origin',(-1.,0.,7.));
#4593=CARTESIAN_POINT('',(-0.285822151001587,-1.23689326713883E-16,7.71417784899841));
#4594=CARTESIAN_POINT('Origin',(-1.,0.,7.));
#4595=CARTESIAN_POINT('Origin',(-1.,0.,7.));
#4596=CARTESIAN_POINT('',(-1.12609520212919,-0.77987178433381,6.87390479787082));
#4597=CARTESIAN_POINT('Origin',(-1.,0.,7.));
#4598=CARTESIAN_POINT('',(-1.12609520212919,0.77987178433381,6.87390479787082));
#4599=CARTESIAN_POINT('Origin',(-1.,0.,7.));
#4600=CARTESIAN_POINT('Origin',(-1.,0.,7.));
#4601=CARTESIAN_POINT('Origin',(-4.6,0.,7.));
#4602=CARTESIAN_POINT('',(-3.1,9.67470971326409E-17,7.79));
#4603=CARTESIAN_POINT('Origin',(-3.1,0.,7.));
#4604=CARTESIAN_POINT('',(-1.90705627484771,-9.67470971326409E-17,7.79));
#4605=CARTESIAN_POINT('',(-4.6,-9.67470971326409E-17,7.79));
#4606=CARTESIAN_POINT('',(-2.20660681251185,-0.619321665126014,7.49044946233587));
#4607=CARTESIAN_POINT('Origin',(-2.69705627484771,0.,7.));
#4608=CARTESIAN_POINT('Ctrl Pts',(-2.20660681251185,-0.619321665126014,
7.49044946233587));
#4609=CARTESIAN_POINT('Ctrl Pts',(-2.18635739895495,-0.626088765992065,
7.48190421456156));
#4610=CARTESIAN_POINT('Ctrl Pts',(-2.1659929610671,-0.632612788451439,7.47330243874781));
#4611=CARTESIAN_POINT('Ctrl Pts',(-2.00496309821175,-0.682136063507274,
7.40520943133101));
#4612=CARTESIAN_POINT('Ctrl Pts',(-1.86106460441583,-0.713835552448689,
7.34397872871663));
#4613=CARTESIAN_POINT('Ctrl Pts',(-1.61917783401457,-0.754887388656086,
7.23855919060182));
#4614=CARTESIAN_POINT('Ctrl Pts',(-1.48614163670725,-0.771174999515586,
7.18006855577991));
#4615=CARTESIAN_POINT('Ctrl Pts',(-1.34421273277038,-0.782619307675673,
7.10904467456489));
#4616=CARTESIAN_POINT('Ctrl Pts',(-1.30795462851338,-0.78510876895878,7.09020452262876));
#4617=CARTESIAN_POINT('Ctrl Pts',(-1.23823362074948,-0.788767674427645,
7.04876648497192));
#4618=CARTESIAN_POINT('Ctrl Pts',(-1.20466978693098,-0.79,7.02634424192971));
#4619=CARTESIAN_POINT('Ctrl Pts',(-1.17832554500127,-0.79,7.));
#4620=CARTESIAN_POINT('Ctrl Pts',(-1.16484458907882,-0.79,6.98651904407755));
#4621=CARTESIAN_POINT('Ctrl Pts',(-1.15267227667281,-0.789658839214769,
6.97115565787718));
#4622=CARTESIAN_POINT('Ctrl Pts',(-1.13503745407884,-0.787668068667849,
6.93697581829037));
#4623=CARTESIAN_POINT('Ctrl Pts',(-1.12967754955442,-0.785984756040963,
6.91810849353946));
#4624=CARTESIAN_POINT('Ctrl Pts',(-1.12651114233652,-0.782433142969531,
6.89060638382703));
#4625=CARTESIAN_POINT('Ctrl Pts',(-1.12609520212919,-0.781224978053133,
6.88227401083545));
#4626=CARTESIAN_POINT('Ctrl Pts',(-1.12609520212919,-0.77987178433381,6.87390479787082));
#4627=CARTESIAN_POINT('',(-2.20660681251185,0.619321665126014,7.49044946233587));
#4628=CARTESIAN_POINT('Ctrl Pts',(-1.12609520212919,0.77987178433381,6.87390479787082));
#4629=CARTESIAN_POINT('Ctrl Pts',(-1.12609520212919,0.781224978053133,6.88227401083545));
#4630=CARTESIAN_POINT('Ctrl Pts',(-1.12651114233652,0.782433142969531,6.89060638382703));
#4631=CARTESIAN_POINT('Ctrl Pts',(-1.12967754955442,0.785984756040963,6.91810849353946));
#4632=CARTESIAN_POINT('Ctrl Pts',(-1.13503745407884,0.787668068667849,6.93697581829037));
#4633=CARTESIAN_POINT('Ctrl Pts',(-1.15267227667281,0.789658839214769,6.97115565787718));
#4634=CARTESIAN_POINT('Ctrl Pts',(-1.16484458907882,0.79,6.98651904407755));
#4635=CARTESIAN_POINT('Ctrl Pts',(-1.20466978693098,0.79,7.02634424192971));
#4636=CARTESIAN_POINT('Ctrl Pts',(-1.23823362074948,0.788767674427645,7.04876648497192));
#4637=CARTESIAN_POINT('Ctrl Pts',(-1.30795462851338,0.78510876895878,7.09020452262876));
#4638=CARTESIAN_POINT('Ctrl Pts',(-1.34421273277038,0.782619307675673,7.10904467456489));
#4639=CARTESIAN_POINT('Ctrl Pts',(-1.48614163670725,0.771174999515586,7.18006855577991));
#4640=CARTESIAN_POINT('Ctrl Pts',(-1.61917783401457,0.754887388656086,7.23855919060182));
#4641=CARTESIAN_POINT('Ctrl Pts',(-1.86106460441583,0.713835552448689,7.34397872871663));
#4642=CARTESIAN_POINT('Ctrl Pts',(-2.00496309821175,0.682136063507274,7.40520943133101));
#4643=CARTESIAN_POINT('Ctrl Pts',(-2.1659929610671,0.632612788451438,7.47330243874781));
#4644=CARTESIAN_POINT('Ctrl Pts',(-2.18635739895495,0.626088765992065,7.48190421456155));
#4645=CARTESIAN_POINT('Ctrl Pts',(-2.20660681251185,0.619321665126014,7.49044946233587));
#4646=CARTESIAN_POINT('Origin',(-2.69705627484771,0.,7.));
#4647=CARTESIAN_POINT('Origin',(-1.84852813742386,0.,7.84852813742386));
#4648=CARTESIAN_POINT('Origin',(-1.84852813742386,0.,7.84852813742386));
#4649=CARTESIAN_POINT('Origin',(-1.84852813742386,0.,7.84852813742386));
#4650=CARTESIAN_POINT('Origin',(3.1,0.,7.));
#4651=CARTESIAN_POINT('',(3.1,-1.13892152320704E-16,7.93));
#4652=CARTESIAN_POINT('Origin',(3.1,0.,7.));
#4653=CARTESIAN_POINT('',(4.5,1.13892152320704E-16,7.93));
#4654=CARTESIAN_POINT('',(3.1,-1.13892152320704E-16,7.93));
#4655=CARTESIAN_POINT('Origin',(4.5,0.,7.));
#4656=CARTESIAN_POINT('Origin',(3.1,0.,7.));
#4657=CARTESIAN_POINT('',(3.1,-9.67470971326409E-17,7.79));
#4658=CARTESIAN_POINT('Origin',(3.1,0.,7.));
#4659=CARTESIAN_POINT('Origin',(-4.6,0.,7.));
#4660=CARTESIAN_POINT('',(-4.5,-1.13892152320704E-16,7.93));
#4661=CARTESIAN_POINT('Origin',(-4.5,0.,7.));
#4662=CARTESIAN_POINT('',(-3.1,-1.13892152320704E-16,7.93));
#4663=CARTESIAN_POINT('',(-4.6,-1.13892152320704E-16,7.93));
#4664=CARTESIAN_POINT('Origin',(-3.1,0.,7.));
#4665=CARTESIAN_POINT('Origin',(-3.1,0.,7.));
#4666=CARTESIAN_POINT('Origin',(0.5,0.,7.));
#4667=CARTESIAN_POINT('',(0.5,-9.67470971326409E-17,7.79));
#4668=CARTESIAN_POINT('Origin',(3.3840620433566,0.,2.61593795664341));
#4669=CARTESIAN_POINT('',(5.50538238691624,-3.67394039744206E-16,4.73725830020305));
#4670=CARTESIAN_POINT('Origin',(3.3840620433566,0.,2.61593795664341));
#4671=CARTESIAN_POINT('',(4.79827560572969,2.44929359829471E-16,4.0301515190165));
#4672=CARTESIAN_POINT('Origin',(3.3840620433566,0.,2.61593795664341));
#4673=CARTESIAN_POINT('Origin',(3.3840620433566,0.,2.61593795664341));
#4674=CARTESIAN_POINT('',(6.07106781186548,-3.67394039744206E-16,4.17157287525381));
#4675=CARTESIAN_POINT('Origin',(3.94974746830583,0.,2.05025253169417));
#4676=CARTESIAN_POINT('',(5.50538238691624,-3.67394039744206E-16,4.73725830020305));
#4677=CARTESIAN_POINT('Origin',(-1.,0.,7.));
#4678=CARTESIAN_POINT('',(3.82842712474619,-2.44929359829471E-16,5.));
#4679=CARTESIAN_POINT('',(0.414213562373095,-2.44929359829471E-16,8.4142135623731));
#4680=CARTESIAN_POINT('',(-1.,-2.,7.));
#4681=CARTESIAN_POINT('Origin',(-1.,0.,7.));
#4682=CARTESIAN_POINT('',(-1.,2.,7.));
#4683=CARTESIAN_POINT('Origin',(-1.,0.,7.));
#4684=CARTESIAN_POINT('Origin',(-1.,0.,7.));
#4685=CARTESIAN_POINT('Origin',(3.94974746830583,0.,2.05025253169417));
#4686=CARTESIAN_POINT('Origin',(-4.5,0.,7.));
#4687=CARTESIAN_POINT('',(4.5,-2.44929359829471E-16,9.));
#4688=CARTESIAN_POINT('Origin',(4.5,0.,7.));
#4689=CARTESIAN_POINT('',(-4.5,-2.44929359829471E-16,9.));
#4690=CARTESIAN_POINT('',(-4.5,-2.44929359829471E-16,9.));
#4691=CARTESIAN_POINT('Origin',(-4.5,0.,7.));
#4692=CARTESIAN_POINT('Origin',(4.5,0.,7.));
#4693=CARTESIAN_POINT('Origin',(-4.5,0.,7.));
#4694=CARTESIAN_POINT('',(0.,0.,0.));
#4695=CARTESIAN_POINT('Origin',(2.50121933088198,-0.848528137423857,2.29878066911802));
#4696=CARTESIAN_POINT('',(2.60349677337681,-0.845307347360138,2.40105811161286));
#4697=CARTESIAN_POINT('',(2.62193000900063,-0.777817459305202,2.27806999099937));
#4698=CARTESIAN_POINT('Ctrl Pts',(2.60349677337681,-0.845307347360138,2.40105811161286));
#4699=CARTESIAN_POINT('Ctrl Pts',(2.61238063875082,-0.845307347360138,2.39217424623885));
#4700=CARTESIAN_POINT('Ctrl Pts',(2.62047795042879,-0.843699478096002,2.38132625304099));
#4701=CARTESIAN_POINT('Ctrl Pts',(2.63236422027647,-0.837090012141717,2.35837214228931));
#4702=CARTESIAN_POINT('Ctrl Pts',(2.63616004051412,-0.832079840080031,2.34627204902667));
#4703=CARTESIAN_POINT('Ctrl Pts',(2.63926437576085,-0.820337643172961,2.32427507285084));
#4704=CARTESIAN_POINT('Ctrl Pts',(2.63878126371775,-0.812819819637263,2.31290975830882));
#4705=CARTESIAN_POINT('Ctrl Pts',(2.63325222648108,-0.796006166512776,2.29294509265423));
#4706=CARTESIAN_POINT('Ctrl Pts',(2.62821183586942,-0.786701304059523,2.28435181786816));
#4707=CARTESIAN_POINT('Ctrl Pts',(2.62193000900063,-0.777817459305202,2.27806999099937));
#4708=CARTESIAN_POINT('Ctrl Pts',(2.62193000900063,-0.777817459305203,2.27806999099937));
#4709=CARTESIAN_POINT('Ctrl Pts',(2.61564818213184,-0.768933614550882,2.27178816413058));
#4710=CARTESIAN_POINT('Ctrl Pts',(2.60729220870594,-0.759293157295718,2.26698507487908));
#4711=CARTESIAN_POINT('Ctrl Pts',(2.58818534635613,-0.741266387103757,2.2623138409472));
#4712=CARTESIAN_POINT('Ctrl Pts',(2.57742834110482,-0.732888284319023,2.2624390381948));
#4713=CARTESIAN_POINT('Ctrl Pts',(2.55657469833452,-0.719529169803534,2.26668670684707));
#4714=CARTESIAN_POINT('Ctrl Pts',(2.54508401494464,-0.713657162034742,2.27109193695749));
#4715=CARTESIAN_POINT('Ctrl Pts',(2.52299022644867,-0.705831016678427,2.28383852906087));
#4716=CARTESIAN_POINT('Ctrl Pts',(2.51238063875082,-0.703885991122829,2.29217424623885));
#4717=CARTESIAN_POINT('Ctrl Pts',(2.49461290800281,-0.703885991122829,2.30994197698686));
#4718=CARTESIAN_POINT('Ctrl Pts',(2.48627719082482,-0.705831016678427,2.32055156468471));
#4719=CARTESIAN_POINT('Ctrl Pts',(2.47353059872144,-0.713657162034742,2.34264535318069));
#4720=CARTESIAN_POINT('Ctrl Pts',(2.46912536861102,-0.719529169803534,2.35413603657057));
#4721=CARTESIAN_POINT('Ctrl Pts',(2.46487769995875,-0.732888284319023,2.37498967934086));
#4722=CARTESIAN_POINT('Ctrl Pts',(2.46475250271115,-0.741266387103756,2.38574668459218));
#4723=CARTESIAN_POINT('Ctrl Pts',(2.46942373664303,-0.759293157295718,2.40485354694198));
#4724=CARTESIAN_POINT('Ctrl Pts',(2.47422682589453,-0.768933614550882,2.41320952036789));
#4725=CARTESIAN_POINT('Ctrl Pts',(2.48679047963211,-0.786701304059523,2.42577317410547));
#4726=CARTESIAN_POINT('Ctrl Pts',(2.49538375441818,-0.796006166512776,2.43081356471713));
#4727=CARTESIAN_POINT('Ctrl Pts',(2.51534842007277,-0.812819819637263,2.4363426019538));
#4728=CARTESIAN_POINT('Ctrl Pts',(2.52671373461479,-0.820337643172961,2.4368257139969));
#4729=CARTESIAN_POINT('Ctrl Pts',(2.54871071079062,-0.832079840080031,2.43372137875017));
#4730=CARTESIAN_POINT('Ctrl Pts',(2.56081080405326,-0.837090012141717,2.42992555851251));
#4731=CARTESIAN_POINT('Ctrl Pts',(2.58376491480494,-0.843699478096002,2.41803928866484));
#4732=CARTESIAN_POINT('Ctrl Pts',(2.5946129080028,-0.845307347360138,2.40994197698686));
#4733=CARTESIAN_POINT('Ctrl Pts',(2.60349677337681,-0.845307347360138,2.40105811161286));
#4734=CARTESIAN_POINT('',(2.67193000900063,-0.707106781186548,2.32806999099937));
#4735=CARTESIAN_POINT('',(2.57193000900063,-0.848528137423857,2.22806999099937));
#4736=CARTESIAN_POINT('',(2.65372561232867,-0.774273042092169,2.45128695056472));
#4737=CARTESIAN_POINT('Ctrl Pts',(2.65372561232867,-0.774273042092169,2.45128695056471));
#4738=CARTESIAN_POINT('Ctrl Pts',(2.64484063125603,-0.774273042092169,2.46017193163735));
#4739=CARTESIAN_POINT('Ctrl Pts',(2.63397978299246,-0.772681811266156,2.46825733795076));
#4740=CARTESIAN_POINT('Ctrl Pts',(2.61098237166811,-0.766133383144486,2.48009968474681));
#4741=CARTESIAN_POINT('Ctrl Pts',(2.59885243375108,-0.761166746032619,2.48386426707181));
#4742=CARTESIAN_POINT('Ctrl Pts',(2.57680007649903,-0.749506871777695,2.48691087693492));
#4743=CARTESIAN_POINT('Ctrl Pts',(2.56540493892266,-0.742032846767245,2.48639760946747));
#4744=CARTESIAN_POINT('Ctrl Pts',(2.54539719598681,-0.725280259543277,2.48082614130759));
#4745=CARTESIAN_POINT('Ctrl Pts',(2.53679126174594,-0.715991732016857,2.4757739562193));
#4746=CARTESIAN_POINT('Ctrl Pts',(2.5242260437807,-0.698221830356238,2.46320873825406));
#4747=CARTESIAN_POINT('Ctrl Pts',(2.51943493755582,-0.688564081560338,2.4548638828766));
#4748=CARTESIAN_POINT('Ctrl Pts',(2.51480720691532,-0.67047684793714,2.43579987746013));
#4749=CARTESIAN_POINT('Ctrl Pts',(2.51496320820213,-0.662056333977536,2.42507400863802));
#4750=CARTESIAN_POINT('Ctrl Pts',(2.51926791560627,-0.648617241117307,2.404279748927));
#4751=CARTESIAN_POINT('Ctrl Pts',(2.52370323294579,-0.642702041451141,2.39282054602449));
#4752=CARTESIAN_POINT('Ctrl Pts',(2.53649267407505,-0.634814219678611,2.37077022903335));
#4753=CARTESIAN_POINT('Ctrl Pts',(2.54484063125604,-0.63285168585486,2.36017193163735));
#4754=CARTESIAN_POINT('Ctrl Pts',(2.5626105934013,-0.63285168585486,2.34240196949208));
#4755=CARTESIAN_POINT('Ctrl Pts',(2.5732088907973,-0.634814219678611,2.33405401231109));
#4756=CARTESIAN_POINT('Ctrl Pts',(2.59525920778845,-0.642702041451141,2.32126457118184));
#4757=CARTESIAN_POINT('Ctrl Pts',(2.60671841069096,-0.648617241117307,2.31682925384232));
#4758=CARTESIAN_POINT('Ctrl Pts',(2.62751267040197,-0.662056333977536,2.31252454643818));
#4759=CARTESIAN_POINT('Ctrl Pts',(2.63823853922408,-0.67047684793714,2.31236854515137));
#4760=CARTESIAN_POINT('Ctrl Pts',(2.65730254464055,-0.688564081560338,2.31699627579187));
#4761=CARTESIAN_POINT('Ctrl Pts',(2.66564740001801,-0.698221830356239,2.32178738201675));
#4762=CARTESIAN_POINT('Ctrl Pts',(2.67193000900063,-0.707106781186548,2.32806999099937));
#4763=CARTESIAN_POINT('Ctrl Pts',(2.67193000900063,-0.707106781186548,2.32806999099937));
#4764=CARTESIAN_POINT('Ctrl Pts',(2.67821261798325,-0.715991732016857,2.33435259998199));
#4765=CARTESIAN_POINT('Ctrl Pts',(2.68326480307154,-0.725280259543277,2.34295853422286));
#4766=CARTESIAN_POINT('Ctrl Pts',(2.68883627123142,-0.742032846767244,2.36296627715871));
#4767=CARTESIAN_POINT('Ctrl Pts',(2.68934953869888,-0.749506871777695,2.37436141473508));
#4768=CARTESIAN_POINT('Ctrl Pts',(2.68630292883576,-0.761166746032619,2.39641377198712));
#4769=CARTESIAN_POINT('Ctrl Pts',(2.68253834651076,-0.766133383144486,2.40854370990416));
#4770=CARTESIAN_POINT('Ctrl Pts',(2.67069599971471,-0.772681811266156,2.4315411212285));
#4771=CARTESIAN_POINT('Ctrl Pts',(2.6626105934013,-0.774273042092169,2.44240196949208));
#4772=CARTESIAN_POINT('Ctrl Pts',(2.65372561232867,-0.774273042092169,2.45128695056471));
#4773=CARTESIAN_POINT('Origin',(2.50121933088198,-0.848528137423857,2.29878066911802));
#4774=CARTESIAN_POINT('',(3.64871304943529,0.63285168585486,3.44627438767133));
#4775=CARTESIAN_POINT('',(3.67193000900063,0.707106781186548,3.32806999099937));
#4776=CARTESIAN_POINT('Ctrl Pts',(3.64871304943529,0.63285168585486,3.44627438767133));
#4777=CARTESIAN_POINT('Ctrl Pts',(3.65759803050792,0.63285168585486,3.4373894065987));
#4778=CARTESIAN_POINT('Ctrl Pts',(3.66594598768891,0.634814219678611,3.4267911092027));
#4779=CARTESIAN_POINT('Ctrl Pts',(3.67873542881816,0.642702041451141,3.40474079221156));
#4780=CARTESIAN_POINT('Ctrl Pts',(3.68317074615768,0.648617241117307,3.39328158930905));
#4781=CARTESIAN_POINT('Ctrl Pts',(3.68747545356182,0.662056333977536,3.37248732959803));
#4782=CARTESIAN_POINT('Ctrl Pts',(3.68763145484863,0.67047684793714,3.36176146077592));
#4783=CARTESIAN_POINT('Ctrl Pts',(3.68300372420813,0.688564081560338,3.34269745535945));
#4784=CARTESIAN_POINT('Ctrl Pts',(3.67821261798325,0.698221830356238,3.33435259998199));
#4785=CARTESIAN_POINT('Ctrl Pts',(3.67193000900063,0.707106781186548,3.32806999099937));
#4786=CARTESIAN_POINT('Ctrl Pts',(3.67193000900063,0.707106781186547,3.32806999099937));
#4787=CARTESIAN_POINT('Ctrl Pts',(3.66564740001801,0.715991732016857,3.32178738201675));
#4788=CARTESIAN_POINT('Ctrl Pts',(3.65704146577714,0.725280259543277,3.31673519692846));
#4789=CARTESIAN_POINT('Ctrl Pts',(3.63703372284129,0.742032846767245,3.31116372876858));
#4790=CARTESIAN_POINT('Ctrl Pts',(3.62563858526492,0.749506871777695,3.31065046130113));
#4791=CARTESIAN_POINT('Ctrl Pts',(3.60358622801288,0.761166746032619,3.31369707116424));
#4792=CARTESIAN_POINT('Ctrl Pts',(3.59145629009584,0.766133383144485,3.31746165348924));
#4793=CARTESIAN_POINT('Ctrl Pts',(3.5684588787715,0.772681811266156,3.32930400028529));
#4794=CARTESIAN_POINT('Ctrl Pts',(3.55759803050792,0.774273042092169,3.3373894065987));
#4795=CARTESIAN_POINT('Ctrl Pts',(3.53982806836266,0.774273042092169,3.35515936874397));
#4796=CARTESIAN_POINT('Ctrl Pts',(3.53174266204924,0.772681811266156,3.36602021700755));
#4797=CARTESIAN_POINT('Ctrl Pts',(3.51990031525319,0.766133383144486,3.38901762833189));
#4798=CARTESIAN_POINT('Ctrl Pts',(3.51613573292819,0.761166746032619,3.40114756624893));
#4799=CARTESIAN_POINT('Ctrl Pts',(3.51308912306508,0.749506871777695,3.42319992350097));
#4800=CARTESIAN_POINT('Ctrl Pts',(3.51360239053253,0.742032846767245,3.43459506107734));
#4801=CARTESIAN_POINT('Ctrl Pts',(3.51917385869241,0.725280259543277,3.45460280401319));
#4802=CARTESIAN_POINT('Ctrl Pts',(3.5242260437807,0.715991732016857,3.46320873825406));
#4803=CARTESIAN_POINT('Ctrl Pts',(3.53679126174594,0.698221830356238,3.4757739562193));
#4804=CARTESIAN_POINT('Ctrl Pts',(3.5451361171234,0.688564081560338,3.48056506244418));
#4805=CARTESIAN_POINT('Ctrl Pts',(3.56420012253987,0.67047684793714,3.48519279308468));
#4806=CARTESIAN_POINT('Ctrl Pts',(3.57492599136198,0.662056333977536,3.48503679179787));
#4807=CARTESIAN_POINT('Ctrl Pts',(3.595720251073,0.648617241117307,3.48073208439373));
#4808=CARTESIAN_POINT('Ctrl Pts',(3.60717945397551,0.642702041451141,3.47629676705421));
#4809=CARTESIAN_POINT('Ctrl Pts',(3.62922977096665,0.634814219678611,3.46350732592496));
#4810=CARTESIAN_POINT('Ctrl Pts',(3.63982806836265,0.63285168585486,3.45515936874397));
#4811=CARTESIAN_POINT('Ctrl Pts',(3.64871304943529,0.63285168585486,3.44627438767133));
#4812=CARTESIAN_POINT('',(3.72193000900063,0.777817459305204,3.37806999099937));
#4813=CARTESIAN_POINT('',(2.57193000900063,-0.848528137423857,2.22806999099937));
#4814=CARTESIAN_POINT('',(3.69894188838714,0.703885991122829,3.49650322662319));
#4815=CARTESIAN_POINT('Ctrl Pts',(3.69894188838714,0.70388599112283,3.49650322662319));
#4816=CARTESIAN_POINT('Ctrl Pts',(3.69005802301314,0.70388599112283,3.5053870919972));
#4817=CARTESIAN_POINT('Ctrl Pts',(3.67944843531529,0.705831016678427,3.51372280917518));
#4818=CARTESIAN_POINT('Ctrl Pts',(3.65735464681931,0.713657162034742,3.52646940127856));
#4819=CARTESIAN_POINT('Ctrl Pts',(3.64586396342943,0.719529169803534,3.53087463138898));
#4820=CARTESIAN_POINT('Ctrl Pts',(3.62501032065914,0.732888284319023,3.53512230004125));
#4821=CARTESIAN_POINT('Ctrl Pts',(3.61425331540782,0.741266387103757,3.53524749728885));
#4822=CARTESIAN_POINT('Ctrl Pts',(3.59514645305802,0.759293157295718,3.53057626335697));
#4823=CARTESIAN_POINT('Ctrl Pts',(3.58679047963211,0.768933614550882,3.52577317410547));
#4824=CARTESIAN_POINT('Ctrl Pts',(3.57422682589453,0.786701304059523,3.51320952036789));
#4825=CARTESIAN_POINT('Ctrl Pts',(3.56918643528287,0.796006166512776,3.50461624558182));
#4826=CARTESIAN_POINT('Ctrl Pts',(3.5636573980462,0.812819819637263,3.48465157992723));
#4827=CARTESIAN_POINT('Ctrl Pts',(3.5631742860031,0.820337643172961,3.47328626538521));
#4828=CARTESIAN_POINT('Ctrl Pts',(3.56627862124983,0.832079840080031,3.45128928920938));
#4829=CARTESIAN_POINT('Ctrl Pts',(3.57007444148749,0.837090012141717,3.43918919594674));
#4830=CARTESIAN_POINT('Ctrl Pts',(3.58196071133516,0.843699478096002,3.41623508519506));
#4831=CARTESIAN_POINT('Ctrl Pts',(3.59005802301314,0.845307347360138,3.4053870919972));
#4832=CARTESIAN_POINT('Ctrl Pts',(3.60782575376115,0.845307347360138,3.38761936124919));
#4833=CARTESIAN_POINT('Ctrl Pts',(3.61867374695901,0.843699478096002,3.37952204957121));
#4834=CARTESIAN_POINT('Ctrl Pts',(3.64162785771069,0.837090012141717,3.36763577972354));
#4835=CARTESIAN_POINT('Ctrl Pts',(3.65372795097333,0.832079840080031,3.36383995948588));
#4836=CARTESIAN_POINT('Ctrl Pts',(3.67572492714916,0.820337643172961,3.36073562423915));
#4837=CARTESIAN_POINT('Ctrl Pts',(3.68709024169119,0.812819819637262,3.36121873628225));
#4838=CARTESIAN_POINT('Ctrl Pts',(3.70705490734577,0.796006166512775,3.36674777351892));
#4839=CARTESIAN_POINT('Ctrl Pts',(3.71564818213184,0.786701304059524,3.37178816413058));
#4840=CARTESIAN_POINT('Ctrl Pts',(3.72193000900063,0.777817459305203,3.37806999099937));
#4841=CARTESIAN_POINT('Ctrl Pts',(3.72193000900063,0.777817459305203,3.37806999099937));
#4842=CARTESIAN_POINT('Ctrl Pts',(3.72821183586942,0.768933614550882,3.38435181786816));
#4843=CARTESIAN_POINT('Ctrl Pts',(3.73301492512092,0.759293157295718,3.39270779129407));
#4844=CARTESIAN_POINT('Ctrl Pts',(3.7376861590528,0.741266387103757,3.41181465364387));
#4845=CARTESIAN_POINT('Ctrl Pts',(3.7375609618052,0.732888284319023,3.42257165889519));
#4846=CARTESIAN_POINT('Ctrl Pts',(3.73331329315294,0.719529169803534,3.44342530166548));
#4847=CARTESIAN_POINT('Ctrl Pts',(3.72890806304252,0.713657162034742,3.45491598505536));
#4848=CARTESIAN_POINT('Ctrl Pts',(3.71616147093913,0.705831016678427,3.47700977355134));
#4849=CARTESIAN_POINT('Ctrl Pts',(3.70782575376115,0.70388599112283,3.48761936124919));
#4850=CARTESIAN_POINT('Ctrl Pts',(3.69894188838714,0.70388599112283,3.49650322662319));
#4851=CARTESIAN_POINT('Origin',(1.3698484809835,-0.848528137423857,3.4301515190165));
#4852=CARTESIAN_POINT('',(1.47212592347833,-0.845307347360138,3.53242896151133));
#4853=CARTESIAN_POINT('',(1.49055915910216,-0.777817459305202,3.40944084089785));
#4854=CARTESIAN_POINT('Ctrl Pts',(1.47212592347833,-0.845307347360138,3.53242896151133));
#4855=CARTESIAN_POINT('Ctrl Pts',(1.48100978885234,-0.845307347360138,3.52354509613733));
#4856=CARTESIAN_POINT('Ctrl Pts',(1.48910710053031,-0.843699478096003,3.51269710293947));
#4857=CARTESIAN_POINT('Ctrl Pts',(1.50099337037799,-0.837090012141717,3.48974299218779));
#4858=CARTESIAN_POINT('Ctrl Pts',(1.50478919061565,-0.832079840080031,3.47764289892514));
#4859=CARTESIAN_POINT('Ctrl Pts',(1.50789352586237,-0.820337643172961,3.45564592274931));
#4860=CARTESIAN_POINT('Ctrl Pts',(1.50741041381927,-0.812819819637263,3.44428060820729));
#4861=CARTESIAN_POINT('Ctrl Pts',(1.5018813765826,-0.796006166512776,3.4243159425527));
#4862=CARTESIAN_POINT('Ctrl Pts',(1.49684098597094,-0.786701304059523,3.41572266776664));
#4863=CARTESIAN_POINT('Ctrl Pts',(1.49055915910215,-0.777817459305202,3.40944084089785));
#4864=CARTESIAN_POINT('Ctrl Pts',(1.49055915910215,-0.777817459305202,3.40944084089785));
#4865=CARTESIAN_POINT('Ctrl Pts',(1.48427733223337,-0.768933614550881,3.40315901402906));
#4866=CARTESIAN_POINT('Ctrl Pts',(1.47592135880746,-0.759293157295718,3.39835592477756));
#4867=CARTESIAN_POINT('Ctrl Pts',(1.45681449645766,-0.741266387103756,3.39368469084567));
#4868=CARTESIAN_POINT('Ctrl Pts',(1.44605749120634,-0.732888284319023,3.39380988809328));
#4869=CARTESIAN_POINT('Ctrl Pts',(1.42520384843604,-0.719529169803534,3.39805755674554));
#4870=CARTESIAN_POINT('Ctrl Pts',(1.41371316504616,-0.713657162034742,3.40246278685596));
#4871=CARTESIAN_POINT('Ctrl Pts',(1.39161937655019,-0.705831016678427,3.41520937895934));
#4872=CARTESIAN_POINT('Ctrl Pts',(1.38100978885234,-0.703885991122829,3.42354509613733));
#4873=CARTESIAN_POINT('Ctrl Pts',(1.36324205810433,-0.703885991122829,3.44131282688534));
#4874=CARTESIAN_POINT('Ctrl Pts',(1.35490634092634,-0.705831016678427,3.45192241458319));
#4875=CARTESIAN_POINT('Ctrl Pts',(1.34215974882296,-0.713657162034742,3.47401620307916));
#4876=CARTESIAN_POINT('Ctrl Pts',(1.33775451871254,-0.719529169803534,3.48550688646904));
#4877=CARTESIAN_POINT('Ctrl Pts',(1.33350685006028,-0.732888284319023,3.50636052923934));
#4878=CARTESIAN_POINT('Ctrl Pts',(1.33338165281267,-0.741266387103756,3.51711753449066));
#4879=CARTESIAN_POINT('Ctrl Pts',(1.33805288674456,-0.759293157295718,3.53622439684046));
#4880=CARTESIAN_POINT('Ctrl Pts',(1.34285597599606,-0.768933614550882,3.54458037026637));
#4881=CARTESIAN_POINT('Ctrl Pts',(1.35541962973363,-0.786701304059523,3.55714402400394));
#4882=CARTESIAN_POINT('Ctrl Pts',(1.3640129045197,-0.796006166512776,3.5621844146156));
#4883=CARTESIAN_POINT('Ctrl Pts',(1.38397757017429,-0.812819819637263,3.56771345185227));
#4884=CARTESIAN_POINT('Ctrl Pts',(1.39534288471631,-0.820337643172961,3.56819656389538));
#4885=CARTESIAN_POINT('Ctrl Pts',(1.41733986089214,-0.832079840080031,3.56509222864865));
#4886=CARTESIAN_POINT('Ctrl Pts',(1.42943995415479,-0.837090012141717,3.56129640841099));
#4887=CARTESIAN_POINT('Ctrl Pts',(1.45239406490647,-0.843699478096002,3.54941013856331));
#4888=CARTESIAN_POINT('Ctrl Pts',(1.46324205810433,-0.845307347360138,3.54131282688534));
#4889=CARTESIAN_POINT('Ctrl Pts',(1.47212592347833,-0.845307347360138,3.53242896151133));
#4890=CARTESIAN_POINT('',(1.54055915910216,-0.707106781186547,3.45944084089785));
#4891=CARTESIAN_POINT('',(1.44055915910215,-0.848528137423857,3.35944084089785));
#4892=CARTESIAN_POINT('',(1.52235476243019,-0.774273042092169,3.58265780046319));
#4893=CARTESIAN_POINT('Ctrl Pts',(1.52235476243019,-0.774273042092169,3.58265780046319));
#4894=CARTESIAN_POINT('Ctrl Pts',(1.51346978135756,-0.774273042092169,3.59154278153582));
#4895=CARTESIAN_POINT('Ctrl Pts',(1.50260893309398,-0.772681811266156,3.59962818784924));
#4896=CARTESIAN_POINT('Ctrl Pts',(1.47961152176963,-0.766133383144486,3.61147053464529));
#4897=CARTESIAN_POINT('Ctrl Pts',(1.4674815838526,-0.761166746032619,3.61523511697029));
#4898=CARTESIAN_POINT('Ctrl Pts',(1.44542922660056,-0.749506871777695,3.6182817268334));
#4899=CARTESIAN_POINT('Ctrl Pts',(1.43403408902419,-0.742032846767245,3.61776845936595));
#4900=CARTESIAN_POINT('Ctrl Pts',(1.41402634608833,-0.725280259543277,3.61219699120607));
#4901=CARTESIAN_POINT('Ctrl Pts',(1.40542041184747,-0.715991732016857,3.60714480611778));
#4902=CARTESIAN_POINT('Ctrl Pts',(1.39285519388222,-0.698221830356238,3.59457958815253));
#4903=CARTESIAN_POINT('Ctrl Pts',(1.38806408765734,-0.688564081560338,3.58623473277508));
#4904=CARTESIAN_POINT('Ctrl Pts',(1.38343635701684,-0.67047684793714,3.5671707273586));
#4905=CARTESIAN_POINT('Ctrl Pts',(1.38359235830366,-0.662056333977536,3.5564448585365));
#4906=CARTESIAN_POINT('Ctrl Pts',(1.38789706570779,-0.648617241117307,3.53565059882548));
#4907=CARTESIAN_POINT('Ctrl Pts',(1.39233238304732,-0.642702041451141,3.52419139592297));
#4908=CARTESIAN_POINT('Ctrl Pts',(1.40512182417657,-0.634814219678611,3.50214107893183));
#4909=CARTESIAN_POINT('Ctrl Pts',(1.41346978135756,-0.63285168585486,3.49154278153582));
#4910=CARTESIAN_POINT('Ctrl Pts',(1.43123974350282,-0.63285168585486,3.47377281939056));
#4911=CARTESIAN_POINT('Ctrl Pts',(1.44183804089883,-0.634814219678611,3.46542486220957));
#4912=CARTESIAN_POINT('Ctrl Pts',(1.46388835788997,-0.642702041451141,3.45263542108032));
#4913=CARTESIAN_POINT('Ctrl Pts',(1.47534756079248,-0.648617241117307,3.44820010374079));
#4914=CARTESIAN_POINT('Ctrl Pts',(1.4961418205035,-0.662056333977536,3.44389539633666));
#4915=CARTESIAN_POINT('Ctrl Pts',(1.5068676893256,-0.67047684793714,3.44373939504984));
#4916=CARTESIAN_POINT('Ctrl Pts',(1.52593169474208,-0.688564081560338,3.44836712569034));
#4917=CARTESIAN_POINT('Ctrl Pts',(1.53427655011953,-0.698221830356238,3.45315823191523));
#4918=CARTESIAN_POINT('Ctrl Pts',(1.54055915910216,-0.707106781186548,3.45944084089785));
#4919=CARTESIAN_POINT('Ctrl Pts',(1.54055915910216,-0.707106781186548,3.45944084089785));
#4920=CARTESIAN_POINT('Ctrl Pts',(1.54684176808478,-0.715991732016857,3.46572344988047));
#4921=CARTESIAN_POINT('Ctrl Pts',(1.55189395317307,-0.725280259543277,3.47432938412133));
#4922=CARTESIAN_POINT('Ctrl Pts',(1.55746542133295,-0.742032846767245,3.49433712705719));
#4923=CARTESIAN_POINT('Ctrl Pts',(1.5579786888004,-0.749506871777695,3.50573226463356));
#4924=CARTESIAN_POINT('Ctrl Pts',(1.55493207893729,-0.761166746032619,3.5277846218856));
#4925=CARTESIAN_POINT('Ctrl Pts',(1.55116749661229,-0.766133383144486,3.53991455980264));
#4926=CARTESIAN_POINT('Ctrl Pts',(1.53932514981624,-0.772681811266156,3.56291197112698));
#4927=CARTESIAN_POINT('Ctrl Pts',(1.53123974350282,-0.774273042092169,3.57377281939056));
#4928=CARTESIAN_POINT('Ctrl Pts',(1.52235476243019,-0.774273042092169,3.58265780046319));
#4929=CARTESIAN_POINT('Origin',(1.3698484809835,-0.848528137423857,3.4301515190165));
#4930=CARTESIAN_POINT('',(2.51734219953681,0.63285168585486,4.57764523756981));
#4931=CARTESIAN_POINT('',(2.54055915910215,0.707106781186547,4.45944084089785));
#4932=CARTESIAN_POINT('Ctrl Pts',(2.51734219953681,0.63285168585486,4.57764523756981));
#4933=CARTESIAN_POINT('Ctrl Pts',(2.52622718060944,0.63285168585486,4.56876025649718));
#4934=CARTESIAN_POINT('Ctrl Pts',(2.53457513779043,0.634814219678611,4.55816195910118));
#4935=CARTESIAN_POINT('Ctrl Pts',(2.54736457891968,0.642702041451141,4.53611164211003));
#4936=CARTESIAN_POINT('Ctrl Pts',(2.55179989625921,0.648617241117307,4.52465243920752));
#4937=CARTESIAN_POINT('Ctrl Pts',(2.55610460366334,0.662056333977536,4.5038581794965));
#4938=CARTESIAN_POINT('Ctrl Pts',(2.55626060495016,0.67047684793714,4.4931323106744));
#4939=CARTESIAN_POINT('Ctrl Pts',(2.55163287430966,0.688564081560338,4.47406830525792));
#4940=CARTESIAN_POINT('Ctrl Pts',(2.54684176808478,0.698221830356238,4.46572344988047));
#4941=CARTESIAN_POINT('Ctrl Pts',(2.54055915910216,0.707106781186548,4.45944084089785));
#4942=CARTESIAN_POINT('Ctrl Pts',(2.54055915910215,0.707106781186548,4.45944084089785));
#4943=CARTESIAN_POINT('Ctrl Pts',(2.53427655011953,0.715991732016857,4.45315823191523));
#4944=CARTESIAN_POINT('Ctrl Pts',(2.52567061587867,0.725280259543277,4.44810604682694));
#4945=CARTESIAN_POINT('Ctrl Pts',(2.50566287294281,0.742032846767245,4.44253457866705));
#4946=CARTESIAN_POINT('Ctrl Pts',(2.49426773536644,0.749506871777695,4.4420213111996));
#4947=CARTESIAN_POINT('Ctrl Pts',(2.4722153781144,0.761166746032619,4.44506792106271));
#4948=CARTESIAN_POINT('Ctrl Pts',(2.46008544019737,0.766133383144486,4.44883250338771));
#4949=CARTESIAN_POINT('Ctrl Pts',(2.43708802887302,0.772681811266156,4.46067485018376));
#4950=CARTESIAN_POINT('Ctrl Pts',(2.42622718060944,0.774273042092169,4.46876025649718));
#4951=CARTESIAN_POINT('Ctrl Pts',(2.40845721846418,0.774273042092169,4.48653021864244));
#4952=CARTESIAN_POINT('Ctrl Pts',(2.40037181215076,0.772681811266156,4.49739106690602));
#4953=CARTESIAN_POINT('Ctrl Pts',(2.38852946535471,0.766133383144486,4.52038847823037));
#4954=CARTESIAN_POINT('Ctrl Pts',(2.38476488302971,0.761166746032619,4.5325184161474));
#4955=CARTESIAN_POINT('Ctrl Pts',(2.3817182731666,0.749506871777695,4.55457077339944));
#4956=CARTESIAN_POINT('Ctrl Pts',(2.38223154063405,0.742032846767245,4.56596591097581));
#4957=CARTESIAN_POINT('Ctrl Pts',(2.38780300879394,0.725280259543277,4.58597365391167));
#4958=CARTESIAN_POINT('Ctrl Pts',(2.39285519388222,0.715991732016857,4.59457958815253));
#4959=CARTESIAN_POINT('Ctrl Pts',(2.40542041184747,0.698221830356238,4.60714480611778));
#4960=CARTESIAN_POINT('Ctrl Pts',(2.41376526722492,0.688564081560338,4.61193591234266));
#4961=CARTESIAN_POINT('Ctrl Pts',(2.4328292726414,0.67047684793714,4.61656364298316));
#4962=CARTESIAN_POINT('Ctrl Pts',(2.4435551414635,0.662056333977536,4.61640764169634));
#4963=CARTESIAN_POINT('Ctrl Pts',(2.46434940117452,0.648617241117307,4.61210293429221));
#4964=CARTESIAN_POINT('Ctrl Pts',(2.47580860407703,0.642702041451142,4.60766761695269));
#4965=CARTESIAN_POINT('Ctrl Pts',(2.49785892106817,0.634814219678611,4.59487817582343));
#4966=CARTESIAN_POINT('Ctrl Pts',(2.50845721846418,0.63285168585486,4.58653021864244));
#4967=CARTESIAN_POINT('Ctrl Pts',(2.51734219953681,0.63285168585486,4.57764523756981));
#4968=CARTESIAN_POINT('',(2.59055915910216,0.777817459305203,4.50944084089785));
#4969=CARTESIAN_POINT('',(1.44055915910215,-0.848528137423857,3.35944084089785));
#4970=CARTESIAN_POINT('',(2.56757103848867,0.703885991122829,4.62787407652167));
#4971=CARTESIAN_POINT('Ctrl Pts',(2.56757103848867,0.703885991122829,4.62787407652167));
#4972=CARTESIAN_POINT('Ctrl Pts',(2.55868717311466,0.703885991122829,4.63675794189567));
#4973=CARTESIAN_POINT('Ctrl Pts',(2.54807758541681,0.705831016678427,4.64509365907366));
#4974=CARTESIAN_POINT('Ctrl Pts',(2.52598379692084,0.713657162034742,4.65784025117704));
#4975=CARTESIAN_POINT('Ctrl Pts',(2.51449311353096,0.719529169803534,4.66224548128746));
#4976=CARTESIAN_POINT('Ctrl Pts',(2.49363947076066,0.732888284319023,4.66649314993972));
#4977=CARTESIAN_POINT('Ctrl Pts',(2.48288246550934,0.741266387103757,4.66661834718733));
#4978=CARTESIAN_POINT('Ctrl Pts',(2.46377560315954,0.759293157295718,4.66194711325544));
#4979=CARTESIAN_POINT('Ctrl Pts',(2.45541962973363,0.768933614550882,4.65714402400394));
#4980=CARTESIAN_POINT('Ctrl Pts',(2.44285597599606,0.786701304059523,4.64458037026637));
#4981=CARTESIAN_POINT('Ctrl Pts',(2.4378155853844,0.796006166512776,4.6359870954803));
#4982=CARTESIAN_POINT('Ctrl Pts',(2.43228654814773,0.812819819637263,4.61602242982571));
#4983=CARTESIAN_POINT('Ctrl Pts',(2.43180343610462,0.820337643172961,4.60465711528369));
#4984=CARTESIAN_POINT('Ctrl Pts',(2.43490777135135,0.832079840080031,4.58266013910786));
#4985=CARTESIAN_POINT('Ctrl Pts',(2.43870359158901,0.837090012141717,4.57056004584521));
#4986=CARTESIAN_POINT('Ctrl Pts',(2.45058986143669,0.843699478096002,4.54760593509353));
#4987=CARTESIAN_POINT('Ctrl Pts',(2.45868717311466,0.845307347360138,4.53675794189567));
#4988=CARTESIAN_POINT('Ctrl Pts',(2.47645490386267,0.845307347360138,4.51899021114766));
#4989=CARTESIAN_POINT('Ctrl Pts',(2.48730289706053,0.843699478096002,4.51089289946969));
#4990=CARTESIAN_POINT('Ctrl Pts',(2.51025700781221,0.837090012141717,4.49900662962201));
#4991=CARTESIAN_POINT('Ctrl Pts',(2.52235710107486,0.832079840080031,4.49521080938436));
#4992=CARTESIAN_POINT('Ctrl Pts',(2.54435407725069,0.820337643172961,4.49210647413763));
#4993=CARTESIAN_POINT('Ctrl Pts',(2.55571939179271,0.812819819637263,4.49258958618073));
#4994=CARTESIAN_POINT('Ctrl Pts',(2.5756840574473,0.796006166512776,4.4981186234174));
#4995=CARTESIAN_POINT('Ctrl Pts',(2.58427733223337,0.786701304059524,4.50315901402906));
#4996=CARTESIAN_POINT('Ctrl Pts',(2.59055915910215,0.777817459305203,4.50944084089785));
#4997=CARTESIAN_POINT('Ctrl Pts',(2.59055915910216,0.777817459305203,4.50944084089785));
#4998=CARTESIAN_POINT('Ctrl Pts',(2.59684098597094,0.768933614550882,4.51572266776664));
#4999=CARTESIAN_POINT('Ctrl Pts',(2.60164407522244,0.759293157295718,4.52407864119254));
#5000=CARTESIAN_POINT('Ctrl Pts',(2.60631530915433,0.741266387103756,4.54318550354234));
#5001=CARTESIAN_POINT('Ctrl Pts',(2.60619011190672,0.732888284319023,4.55394250879366));
#5002=CARTESIAN_POINT('Ctrl Pts',(2.60194244325446,0.719529169803535,4.57479615156396));
#5003=CARTESIAN_POINT('Ctrl Pts',(2.59753721314404,0.713657162034742,4.58628683495384));
#5004=CARTESIAN_POINT('Ctrl Pts',(2.58479062104066,0.705831016678427,4.60838062344981));
#5005=CARTESIAN_POINT('Ctrl Pts',(2.57645490386267,0.703885991122829,4.61899021114766));
#5006=CARTESIAN_POINT('Ctrl Pts',(2.56757103848867,0.703885991122829,4.62787407652167));
#5007=CARTESIAN_POINT('Origin',(0.804163056034262,-0.848528137423857,3.99583694396574));
#5008=CARTESIAN_POINT('',(0.906440498529096,-0.845307347360138,4.09811438646057));
#5009=CARTESIAN_POINT('',(0.924873734152917,-0.777817459305202,3.97512626584708));
#5010=CARTESIAN_POINT('Ctrl Pts',(0.906440498529096,-0.845307347360138,
4.09811438646057));
#5011=CARTESIAN_POINT('Ctrl Pts',(0.915324363903102,-0.845307347360138,
4.08923052108657));
#5012=CARTESIAN_POINT('Ctrl Pts',(0.923421675581074,-0.843699478096003,
4.07838252788871));
#5013=CARTESIAN_POINT('Ctrl Pts',(0.935307945428751,-0.837090012141717,
4.05542841713702));
#5014=CARTESIAN_POINT('Ctrl Pts',(0.939103765666409,-0.832079840080031,
4.04332832387438));
#5015=CARTESIAN_POINT('Ctrl Pts',(0.942208100913137,-0.820337643172961,
4.02133134769855));
#5016=CARTESIAN_POINT('Ctrl Pts',(0.941724988870036,-0.812819819637263,
4.00996603315653));
#5017=CARTESIAN_POINT('Ctrl Pts',(0.936195951633367,-0.796006166512776,
3.99000136750194));
#5018=CARTESIAN_POINT('Ctrl Pts',(0.931155561021706,-0.786701304059524,
3.98140809271587));
#5019=CARTESIAN_POINT('Ctrl Pts',(0.924873734152917,-0.777817459305203,
3.97512626584708));
#5020=CARTESIAN_POINT('Ctrl Pts',(0.924873734152917,-0.777817459305202,
3.97512626584708));
#5021=CARTESIAN_POINT('Ctrl Pts',(0.918591907284128,-0.768933614550881,
3.96884443897829));
#5022=CARTESIAN_POINT('Ctrl Pts',(0.910235933858221,-0.759293157295718,
3.9640413497268));
#5023=CARTESIAN_POINT('Ctrl Pts',(0.891129071508419,-0.741266387103756,
3.95937011579491));
#5024=CARTESIAN_POINT('Ctrl Pts',(0.880372066257102,-0.732888284319023,
3.95949531304252));
#5025=CARTESIAN_POINT('Ctrl Pts',(0.859518423486807,-0.719529169803534,
3.96374298169478));
#5026=CARTESIAN_POINT('Ctrl Pts',(0.848027740096926,-0.713657162034741,
3.9681482118052));
#5027=CARTESIAN_POINT('Ctrl Pts',(0.82593395160095,-0.705831016678426,3.98089480390858));
#5028=CARTESIAN_POINT('Ctrl Pts',(0.815324363903101,-0.703885991122829,
3.98923052108657));
#5029=CARTESIAN_POINT('Ctrl Pts',(0.797556633155091,-0.703885991122829,
4.00699825183458));
#5030=CARTESIAN_POINT('Ctrl Pts',(0.789220915977106,-0.705831016678426,
4.01760783953243));
#5031=CARTESIAN_POINT('Ctrl Pts',(0.776474323873723,-0.713657162034741,
4.0397016280284));
#5032=CARTESIAN_POINT('Ctrl Pts',(0.772069093763303,-0.719529169803534,
4.05119231141828));
#5033=CARTESIAN_POINT('Ctrl Pts',(0.76782142511104,-0.732888284319023,4.07204595418858));
#5034=CARTESIAN_POINT('Ctrl Pts',(0.767696227863436,-0.741266387103756,
4.08280295943989));
#5035=CARTESIAN_POINT('Ctrl Pts',(0.77236746179532,-0.759293157295718,4.1019098217897));
#5036=CARTESIAN_POINT('Ctrl Pts',(0.777170551046818,-0.768933614550882,
4.1102657952156));
#5037=CARTESIAN_POINT('Ctrl Pts',(0.789734204784396,-0.786701304059523,
4.12282944895318));
#5038=CARTESIAN_POINT('Ctrl Pts',(0.798327479570465,-0.796006166512776,
4.12786983956484));
#5039=CARTESIAN_POINT('Ctrl Pts',(0.818292145225052,-0.812819819637263,
4.13339887680151));
#5040=CARTESIAN_POINT('Ctrl Pts',(0.829657459767076,-0.820337643172961,
4.13388198884461));
#5041=CARTESIAN_POINT('Ctrl Pts',(0.851654435942905,-0.832079840080031,
4.13077765359789));
#5042=CARTESIAN_POINT('Ctrl Pts',(0.863754529205548,-0.837090012141717,
4.12698183336023));
#5043=CARTESIAN_POINT('Ctrl Pts',(0.886708639957229,-0.843699478096003,
4.11509556351255));
#5044=CARTESIAN_POINT('Ctrl Pts',(0.89755663315509,-0.845307347360138,4.10699825183458));
#5045=CARTESIAN_POINT('Ctrl Pts',(0.906440498529096,-0.845307347360138,
4.09811438646057));
#5046=CARTESIAN_POINT('',(0.974873734152917,-0.707106781186547,4.02512626584708));
#5047=CARTESIAN_POINT('',(0.874873734152917,-0.848528137423857,3.92512626584708));
#5048=CARTESIAN_POINT('',(0.956669337480952,-0.774273042092169,4.14834322541243));
#5049=CARTESIAN_POINT('Ctrl Pts',(0.956669337480953,-0.774273042092169,
4.14834322541243));
#5050=CARTESIAN_POINT('Ctrl Pts',(0.947784356408321,-0.774273042092169,
4.15722820648506));
#5051=CARTESIAN_POINT('Ctrl Pts',(0.936923508144742,-0.772681811266156,
4.16531361279847));
#5052=CARTESIAN_POINT('Ctrl Pts',(0.913926096820398,-0.766133383144486,
4.17715595959453));
#5053=CARTESIAN_POINT('Ctrl Pts',(0.901796158903362,-0.76116674603262,4.18092054191952));
#5054=CARTESIAN_POINT('Ctrl Pts',(0.879743801651321,-0.749506871777696,
4.18396715178264));
#5055=CARTESIAN_POINT('Ctrl Pts',(0.86834866407495,-0.742032846767245,4.18345388431518));
#5056=CARTESIAN_POINT('Ctrl Pts',(0.848340921139093,-0.725280259543278,
4.1778824161553));
#5057=CARTESIAN_POINT('Ctrl Pts',(0.839734986898228,-0.715991732016857,
4.17283023106701));
#5058=CARTESIAN_POINT('Ctrl Pts',(0.827169768932986,-0.698221830356238,
4.16026501310177));
#5059=CARTESIAN_POINT('Ctrl Pts',(0.822378662708104,-0.688564081560337,
4.15192015772431));
#5060=CARTESIAN_POINT('Ctrl Pts',(0.817750932067606,-0.67047684793714,4.13285615230784));
#5061=CARTESIAN_POINT('Ctrl Pts',(0.817906933354418,-0.662056333977536,
4.12213028348573));
#5062=CARTESIAN_POINT('Ctrl Pts',(0.822211640758555,-0.648617241117306,
4.10133602377472));
#5063=CARTESIAN_POINT('Ctrl Pts',(0.826646958098078,-0.642702041451141,
4.08987682087221));
#5064=CARTESIAN_POINT('Ctrl Pts',(0.839436399227331,-0.634814219678611,
4.06782650388106));
#5065=CARTESIAN_POINT('Ctrl Pts',(0.847784356408321,-0.63285168585486,4.05722820648506));
#5066=CARTESIAN_POINT('Ctrl Pts',(0.865554318553583,-0.63285168585486,4.0394582443398));
#5067=CARTESIAN_POINT('Ctrl Pts',(0.876152615949588,-0.63481421967861,4.03111028715881));
#5068=CARTESIAN_POINT('Ctrl Pts',(0.898202932940732,-0.642702041451141,
4.01832084602955));
#5069=CARTESIAN_POINT('Ctrl Pts',(0.909662135843242,-0.648617241117307,
4.01388552869003));
#5070=CARTESIAN_POINT('Ctrl Pts',(0.930456395554258,-0.662056333977536,
4.00958082128589));
#5071=CARTESIAN_POINT('Ctrl Pts',(0.941182264376365,-0.67047684793714,4.00942481999908));
#5072=CARTESIAN_POINT('Ctrl Pts',(0.960246269792838,-0.688564081560337,
4.01405255063958));
#5073=CARTESIAN_POINT('Ctrl Pts',(0.968591125170296,-0.698221830356238,
4.01884365686446));
#5074=CARTESIAN_POINT('Ctrl Pts',(0.974873734152917,-0.707106781186548,
4.02512626584708));
#5075=CARTESIAN_POINT('Ctrl Pts',(0.974873734152917,-0.707106781186547,
4.02512626584708));
#5076=CARTESIAN_POINT('Ctrl Pts',(0.981156343135538,-0.715991732016857,
4.0314088748297));
#5077=CARTESIAN_POINT('Ctrl Pts',(0.986208528223828,-0.725280259543278,
4.04001480907057));
#5078=CARTESIAN_POINT('Ctrl Pts',(0.991779996383709,-0.742032846767245,
4.06002255200643));
#5079=CARTESIAN_POINT('Ctrl Pts',(0.992293263851161,-0.749506871777695,
4.0714176895828));
#5080=CARTESIAN_POINT('Ctrl Pts',(0.989246653988048,-0.761166746032619,
4.09347004683484));
#5081=CARTESIAN_POINT('Ctrl Pts',(0.98548207166305,-0.766133383144486,4.10559998475187));
#5082=CARTESIAN_POINT('Ctrl Pts',(0.973639724866999,-0.772681811266156,
4.12859739607622));
#5083=CARTESIAN_POINT('Ctrl Pts',(0.965554318553584,-0.774273042092169,
4.1394582443398));
#5084=CARTESIAN_POINT('Ctrl Pts',(0.956669337480953,-0.774273042092169,
4.14834322541243));
#5085=CARTESIAN_POINT('Origin',(0.804163056034262,-0.848528137423857,3.99583694396574));
#5086=CARTESIAN_POINT('',(1.95165677458757,0.63285168585486,5.14333066251905));
#5087=CARTESIAN_POINT('',(1.97487373415292,0.707106781186548,5.02512626584708));
#5088=CARTESIAN_POINT('Ctrl Pts',(1.95165677458757,0.63285168585486,5.14333066251905));
#5089=CARTESIAN_POINT('Ctrl Pts',(1.9605417556602,0.63285168585486,5.13444568144642));
#5090=CARTESIAN_POINT('Ctrl Pts',(1.96888971284119,0.634814219678611,5.12384738405041));
#5091=CARTESIAN_POINT('Ctrl Pts',(1.98167915397045,0.642702041451141,5.10179706705927));
#5092=CARTESIAN_POINT('Ctrl Pts',(1.98611447130997,0.648617241117307,5.09033786415676));
#5093=CARTESIAN_POINT('Ctrl Pts',(1.99041917871411,0.662056333977536,5.06954360444574));
#5094=CARTESIAN_POINT('Ctrl Pts',(1.99057518000092,0.67047684793714,5.05881773562364));
#5095=CARTESIAN_POINT('Ctrl Pts',(1.98594744936042,0.688564081560337,5.03975373020716));
#5096=CARTESIAN_POINT('Ctrl Pts',(1.98115634313554,0.698221830356239,5.0314088748297));
#5097=CARTESIAN_POINT('Ctrl Pts',(1.97487373415292,0.707106781186548,5.02512626584708));
#5098=CARTESIAN_POINT('Ctrl Pts',(1.97487373415292,0.707106781186548,5.02512626584708));
#5099=CARTESIAN_POINT('Ctrl Pts',(1.9685911251703,0.715991732016857,5.01884365686446));
#5100=CARTESIAN_POINT('Ctrl Pts',(1.95998519092943,0.725280259543277,5.01379147177617));
#5101=CARTESIAN_POINT('Ctrl Pts',(1.93997744799358,0.742032846767245,5.00822000361629));
#5102=CARTESIAN_POINT('Ctrl Pts',(1.9285823104172,0.749506871777696,5.00770673614884));
#5103=CARTESIAN_POINT('Ctrl Pts',(1.90652995316516,0.76116674603262,5.01075334601195));
#5104=CARTESIAN_POINT('Ctrl Pts',(1.89440001524813,0.766133383144486,5.01451792833695));
#5105=CARTESIAN_POINT('Ctrl Pts',(1.87140260392378,0.772681811266156,5.026360275133));
#5106=CARTESIAN_POINT('Ctrl Pts',(1.8605417556602,0.77427304209217,5.03444568144642));
#5107=CARTESIAN_POINT('Ctrl Pts',(1.84277179351494,0.77427304209217,5.05221564359168));
#5108=CARTESIAN_POINT('Ctrl Pts',(1.83468638720153,0.772681811266157,5.06307649185526));
#5109=CARTESIAN_POINT('Ctrl Pts',(1.82284404040548,0.766133383144487,5.0860739031796));
#5110=CARTESIAN_POINT('Ctrl Pts',(1.81907945808048,0.76116674603262,5.09820384109664));
#5111=CARTESIAN_POINT('Ctrl Pts',(1.81603284821736,0.749506871777696,5.12025619834868));
#5112=CARTESIAN_POINT('Ctrl Pts',(1.81654611568482,0.742032846767245,5.13165133592505));
#5113=CARTESIAN_POINT('Ctrl Pts',(1.8221175838447,0.725280259543278,5.15165907886091));
#5114=CARTESIAN_POINT('Ctrl Pts',(1.82716976893299,0.715991732016857,5.16026501310177));
#5115=CARTESIAN_POINT('Ctrl Pts',(1.83973498689823,0.698221830356238,5.17283023106701));
#5116=CARTESIAN_POINT('Ctrl Pts',(1.84807984227569,0.688564081560337,5.1776213372919));
#5117=CARTESIAN_POINT('Ctrl Pts',(1.86714384769216,0.67047684793714,5.1822490679324));
#5118=CARTESIAN_POINT('Ctrl Pts',(1.87786971651427,0.662056333977536,5.18209306664558));
#5119=CARTESIAN_POINT('Ctrl Pts',(1.89866397622528,0.648617241117307,5.17778835924145));
#5120=CARTESIAN_POINT('Ctrl Pts',(1.91012317912779,0.64270204145114,5.17335304190192));
#5121=CARTESIAN_POINT('Ctrl Pts',(1.93217349611894,0.63481421967861,5.16056360077267));
#5122=CARTESIAN_POINT('Ctrl Pts',(1.94277179351494,0.63285168585486,5.15221564359168));
#5123=CARTESIAN_POINT('Ctrl Pts',(1.95165677458757,0.63285168585486,5.14333066251905));
#5124=CARTESIAN_POINT('',(2.02487373415292,0.777817459305203,5.07512626584709));
#5125=CARTESIAN_POINT('',(0.874873734152917,-0.848528137423857,3.92512626584708));
#5126=CARTESIAN_POINT('',(2.00188561353943,0.703885991122829,5.1935595014709));
#5127=CARTESIAN_POINT('Ctrl Pts',(2.00188561353943,0.703885991122829,5.19355950147091));
#5128=CARTESIAN_POINT('Ctrl Pts',(1.99300174816542,0.703885991122829,5.20244336684491));
#5129=CARTESIAN_POINT('Ctrl Pts',(1.98239216046757,0.705831016678426,5.2107790840229));
#5130=CARTESIAN_POINT('Ctrl Pts',(1.9602983719716,0.713657162034741,5.22352567612628));
#5131=CARTESIAN_POINT('Ctrl Pts',(1.94880768858172,0.719529169803534,5.2279309062367));
#5132=CARTESIAN_POINT('Ctrl Pts',(1.92795404581142,0.732888284319023,5.23217857488896));
#5133=CARTESIAN_POINT('Ctrl Pts',(1.91719704056011,0.741266387103756,5.23230377213657));
#5134=CARTESIAN_POINT('Ctrl Pts',(1.8980901782103,0.759293157295718,5.22763253820468));
#5135=CARTESIAN_POINT('Ctrl Pts',(1.8897342047844,0.768933614550882,5.22282944895318));
#5136=CARTESIAN_POINT('Ctrl Pts',(1.87717055104682,0.786701304059523,5.21026579521561));
#5137=CARTESIAN_POINT('Ctrl Pts',(1.87213016043516,0.796006166512776,5.20167252042953));
#5138=CARTESIAN_POINT('Ctrl Pts',(1.86660112319849,0.812819819637263,5.18170785477495));
#5139=CARTESIAN_POINT('Ctrl Pts',(1.86611801115539,0.820337643172962,5.17034254023292));
#5140=CARTESIAN_POINT('Ctrl Pts',(1.86922234640212,0.832079840080031,5.1483455640571));
#5141=CARTESIAN_POINT('Ctrl Pts',(1.87301816663977,0.837090012141718,5.13624547079445));
#5142=CARTESIAN_POINT('Ctrl Pts',(1.88490443648745,0.843699478096003,5.11329136004277));
#5143=CARTESIAN_POINT('Ctrl Pts',(1.89300174816542,0.845307347360138,5.10244336684491));
#5144=CARTESIAN_POINT('Ctrl Pts',(1.91076947891343,0.845307347360138,5.0846756360969));
#5145=CARTESIAN_POINT('Ctrl Pts',(1.92161747211129,0.843699478096003,5.07657832441893));
#5146=CARTESIAN_POINT('Ctrl Pts',(1.94457158286298,0.837090012141717,5.06469205457125));
#5147=CARTESIAN_POINT('Ctrl Pts',(1.95667167612562,0.832079840080031,5.06089623433359));
#5148=CARTESIAN_POINT('Ctrl Pts',(1.97866865230145,0.820337643172961,5.05779189908686));
#5149=CARTESIAN_POINT('Ctrl Pts',(1.99003396684347,0.812819819637263,5.05827501112996));
#5150=CARTESIAN_POINT('Ctrl Pts',(2.00999863249806,0.796006166512776,5.06380404836663));
#5151=CARTESIAN_POINT('Ctrl Pts',(2.01859190728413,0.786701304059523,5.0688444389783));
#5152=CARTESIAN_POINT('Ctrl Pts',(2.02487373415292,0.777817459305203,5.07512626584708));
#5153=CARTESIAN_POINT('Ctrl Pts',(2.02487373415292,0.777817459305203,5.07512626584708));
#5154=CARTESIAN_POINT('Ctrl Pts',(2.03115556102171,0.768933614550882,5.08140809271587));
#5155=CARTESIAN_POINT('Ctrl Pts',(2.0359586502732,0.759293157295718,5.08976406614178));
#5156=CARTESIAN_POINT('Ctrl Pts',(2.04062988420509,0.741266387103756,5.10887092849158));
#5157=CARTESIAN_POINT('Ctrl Pts',(2.04050468695748,0.732888284319023,5.1196279337429));
#5158=CARTESIAN_POINT('Ctrl Pts',(2.03625701830522,0.719529169803534,5.14048157651319));
#5159=CARTESIAN_POINT('Ctrl Pts',(2.0318517881948,0.713657162034742,5.15197225990308));
#5160=CARTESIAN_POINT('Ctrl Pts',(2.01910519609142,0.705831016678426,5.17406604839905));
#5161=CARTESIAN_POINT('Ctrl Pts',(2.01076947891343,0.703885991122829,5.1846756360969));
#5162=CARTESIAN_POINT('Ctrl Pts',(2.00188561353943,0.703885991122829,5.19355950147091));
#5163=CARTESIAN_POINT('Origin',(0.238477631085024,-0.848528137423857,4.56152236891498));
#5164=CARTESIAN_POINT('',(0.340755073579858,-0.845307347360138,4.66379981140981));
#5165=CARTESIAN_POINT('',(0.359188309203679,-0.777817459305203,4.54081169079632));
#5166=CARTESIAN_POINT('Ctrl Pts',(0.340755073579858,-0.845307347360138,
4.66379981140981));
#5167=CARTESIAN_POINT('Ctrl Pts',(0.349638938953863,-0.845307347360138,
4.65491594603581));
#5168=CARTESIAN_POINT('Ctrl Pts',(0.357736250631836,-0.843699478096003,
4.64406795283794));
#5169=CARTESIAN_POINT('Ctrl Pts',(0.369622520479513,-0.837090012141717,
4.62111384208626));
#5170=CARTESIAN_POINT('Ctrl Pts',(0.373418340717171,-0.832079840080031,
4.60901374882362));
#5171=CARTESIAN_POINT('Ctrl Pts',(0.3765226759639,-0.820337643172961,4.58701677264779));
#5172=CARTESIAN_POINT('Ctrl Pts',(0.376039563920798,-0.812819819637263,
4.57565145810577));
#5173=CARTESIAN_POINT('Ctrl Pts',(0.37051052668413,-0.796006166512776,4.55568679245118));
#5174=CARTESIAN_POINT('Ctrl Pts',(0.365470136072468,-0.786701304059523,
4.54709351766511));
#5175=CARTESIAN_POINT('Ctrl Pts',(0.359188309203679,-0.777817459305202,
4.54081169079632));
#5176=CARTESIAN_POINT('Ctrl Pts',(0.359188309203678,-0.777817459305202,
4.54081169079632));
#5177=CARTESIAN_POINT('Ctrl Pts',(0.35290648233489,-0.768933614550881,4.53452986392753));
#5178=CARTESIAN_POINT('Ctrl Pts',(0.344550508908983,-0.759293157295718,
4.52972677467603));
#5179=CARTESIAN_POINT('Ctrl Pts',(0.325443646559181,-0.741266387103756,
4.52505554074415));
#5180=CARTESIAN_POINT('Ctrl Pts',(0.314686641307864,-0.732888284319023,
4.52518073799175));
#5181=CARTESIAN_POINT('Ctrl Pts',(0.293832998537568,-0.719529169803534,
4.52942840664402));
#5182=CARTESIAN_POINT('Ctrl Pts',(0.282342315147688,-0.713657162034741,
4.53383363675444));
#5183=CARTESIAN_POINT('Ctrl Pts',(0.260248526651712,-0.705831016678426,
4.54658022885782));
#5184=CARTESIAN_POINT('Ctrl Pts',(0.249638938953864,-0.703885991122829,
4.5549159460358));
#5185=CARTESIAN_POINT('Ctrl Pts',(0.231871208205852,-0.703885991122829,
4.57268367678382));
#5186=CARTESIAN_POINT('Ctrl Pts',(0.223535491027868,-0.705831016678426,
4.58329326448166));
#5187=CARTESIAN_POINT('Ctrl Pts',(0.210788898924485,-0.713657162034741,
4.60538705297764));
#5188=CARTESIAN_POINT('Ctrl Pts',(0.206383668814065,-0.719529169803534,
4.61687773636752));
#5189=CARTESIAN_POINT('Ctrl Pts',(0.202136000161802,-0.732888284319023,
4.63773137913782));
#5190=CARTESIAN_POINT('Ctrl Pts',(0.202010802914197,-0.741266387103756,
4.64848838438913));
#5191=CARTESIAN_POINT('Ctrl Pts',(0.206682036846082,-0.759293157295718,
4.66759524673894));
#5192=CARTESIAN_POINT('Ctrl Pts',(0.211485126097581,-0.768933614550882,
4.67595122016484));
#5193=CARTESIAN_POINT('Ctrl Pts',(0.224048779835158,-0.786701304059523,
4.68851487390242));
#5194=CARTESIAN_POINT('Ctrl Pts',(0.232642054621227,-0.796006166512776,
4.69355526451408));
#5195=CARTESIAN_POINT('Ctrl Pts',(0.252606720275814,-0.812819819637263,
4.69908430175075));
#5196=CARTESIAN_POINT('Ctrl Pts',(0.263972034817838,-0.820337643172961,
4.69956741379385));
#5197=CARTESIAN_POINT('Ctrl Pts',(0.285969010993667,-0.832079840080031,
4.69646307854712));
#5198=CARTESIAN_POINT('Ctrl Pts',(0.29806910425631,-0.837090012141717,4.69266725830947));
#5199=CARTESIAN_POINT('Ctrl Pts',(0.321023215007992,-0.843699478096003,
4.68078098846179));
#5200=CARTESIAN_POINT('Ctrl Pts',(0.331871208205852,-0.845307347360138,
4.67268367678382));
#5201=CARTESIAN_POINT('Ctrl Pts',(0.340755073579858,-0.845307347360138,
4.66379981140981));
#5202=CARTESIAN_POINT('',(0.409188309203679,-0.707106781186548,4.59081169079632));
#5203=CARTESIAN_POINT('',(0.309188309203679,-0.848528137423857,4.49081169079632));
#5204=CARTESIAN_POINT('',(0.390983912531714,-0.774273042092169,4.71402865036167));
#5205=CARTESIAN_POINT('Ctrl Pts',(0.390983912531714,-0.774273042092169,
4.71402865036167));
#5206=CARTESIAN_POINT('Ctrl Pts',(0.382098931459083,-0.774273042092169,
4.7229136314343));
#5207=CARTESIAN_POINT('Ctrl Pts',(0.371238083195504,-0.772681811266156,
4.73099903774771));
#5208=CARTESIAN_POINT('Ctrl Pts',(0.348240671871159,-0.766133383144486,
4.74284138454376));
#5209=CARTESIAN_POINT('Ctrl Pts',(0.336110733954123,-0.76116674603262,4.74660596686876));
#5210=CARTESIAN_POINT('Ctrl Pts',(0.314058376702083,-0.749506871777696,
4.74965257673188));
#5211=CARTESIAN_POINT('Ctrl Pts',(0.302663239125711,-0.742032846767245,
4.74913930926442));
#5212=CARTESIAN_POINT('Ctrl Pts',(0.282655496189856,-0.725280259543277,
4.74356784110454));
#5213=CARTESIAN_POINT('Ctrl Pts',(0.27404956194899,-0.715991732016857,4.73851565601625));
#5214=CARTESIAN_POINT('Ctrl Pts',(0.261484343983749,-0.698221830356238,
4.72595043805101));
#5215=CARTESIAN_POINT('Ctrl Pts',(0.256693237758866,-0.688564081560337,
4.71760558267355));
#5216=CARTESIAN_POINT('Ctrl Pts',(0.252065507118367,-0.67047684793714,4.69854157725708));
#5217=CARTESIAN_POINT('Ctrl Pts',(0.252221508405179,-0.662056333977536,
4.68781570843497));
#5218=CARTESIAN_POINT('Ctrl Pts',(0.256526215809317,-0.648617241117307,
4.66702144872396));
#5219=CARTESIAN_POINT('Ctrl Pts',(0.260961533148841,-0.64270204145114,4.65556224582144));
#5220=CARTESIAN_POINT('Ctrl Pts',(0.273750974278093,-0.63481421967861,4.6335119288303));
#5221=CARTESIAN_POINT('Ctrl Pts',(0.282098931459083,-0.63285168585486,4.6229136314343));
#5222=CARTESIAN_POINT('Ctrl Pts',(0.299868893604346,-0.63285168585486,4.60514366928903));
#5223=CARTESIAN_POINT('Ctrl Pts',(0.310467191000349,-0.63481421967861,4.59679571210804));
#5224=CARTESIAN_POINT('Ctrl Pts',(0.332517507991493,-0.64270204145114,4.58400627097879));
#5225=CARTESIAN_POINT('Ctrl Pts',(0.343976710894004,-0.648617241117307,
4.57957095363927));
#5226=CARTESIAN_POINT('Ctrl Pts',(0.36477097060502,-0.662056333977536,4.57526624623513));
#5227=CARTESIAN_POINT('Ctrl Pts',(0.375496839427127,-0.67047684793714,4.57511024494832));
#5228=CARTESIAN_POINT('Ctrl Pts',(0.394560844843601,-0.688564081560337,
4.57973797558882));
#5229=CARTESIAN_POINT('Ctrl Pts',(0.402905700221058,-0.698221830356238,
4.5845290818137));
#5230=CARTESIAN_POINT('Ctrl Pts',(0.409188309203679,-0.707106781186548,
4.59081169079632));
#5231=CARTESIAN_POINT('Ctrl Pts',(0.409188309203679,-0.707106781186547,
4.59081169079632));
#5232=CARTESIAN_POINT('Ctrl Pts',(0.415470918186299,-0.715991732016857,
4.59709429977894));
#5233=CARTESIAN_POINT('Ctrl Pts',(0.42052310327459,-0.725280259543278,4.60570023401981));
#5234=CARTESIAN_POINT('Ctrl Pts',(0.426094571434471,-0.742032846767245,
4.62570797695566));
#5235=CARTESIAN_POINT('Ctrl Pts',(0.426607838901923,-0.749506871777696,
4.63710311453204));
#5236=CARTESIAN_POINT('Ctrl Pts',(0.42356122903881,-0.76116674603262,4.65915547178408));
#5237=CARTESIAN_POINT('Ctrl Pts',(0.419796646713811,-0.766133383144486,
4.67128540970111));
#5238=CARTESIAN_POINT('Ctrl Pts',(0.407954299917761,-0.772681811266156,
4.69428282102546));
#5239=CARTESIAN_POINT('Ctrl Pts',(0.399868893604345,-0.774273042092169,
4.70514366928904));
#5240=CARTESIAN_POINT('Ctrl Pts',(0.390983912531714,-0.774273042092169,
4.71402865036167));
#5241=CARTESIAN_POINT('Origin',(0.238477631085024,-0.848528137423857,4.56152236891498));
#5242=CARTESIAN_POINT('',(1.38597134963833,0.63285168585486,5.70901608746829));
#5243=CARTESIAN_POINT('',(1.40918830920368,0.707106781186547,5.59081169079632));
#5244=CARTESIAN_POINT('Ctrl Pts',(1.38597134963833,0.632851685854859,5.70901608746829));
#5245=CARTESIAN_POINT('Ctrl Pts',(1.39485633071096,0.632851685854859,5.70013110639566));
#5246=CARTESIAN_POINT('Ctrl Pts',(1.40320428789196,0.63481421967861,5.68953280899965));
#5247=CARTESIAN_POINT('Ctrl Pts',(1.41599372902121,0.642702041451141,5.66748249200851));
#5248=CARTESIAN_POINT('Ctrl Pts',(1.42042904636073,0.648617241117307,5.656023289106));
#5249=CARTESIAN_POINT('Ctrl Pts',(1.42473375376487,0.662056333977536,5.63522902939498));
#5250=CARTESIAN_POINT('Ctrl Pts',(1.42488975505168,0.67047684793714,5.62450316057287));
#5251=CARTESIAN_POINT('Ctrl Pts',(1.42026202441118,0.688564081560337,5.6054391551564));
#5252=CARTESIAN_POINT('Ctrl Pts',(1.4154709181863,0.698221830356238,5.59709429977894));
#5253=CARTESIAN_POINT('Ctrl Pts',(1.40918830920368,0.707106781186548,5.59081169079632));
#5254=CARTESIAN_POINT('Ctrl Pts',(1.40918830920368,0.707106781186548,5.59081169079632));
#5255=CARTESIAN_POINT('Ctrl Pts',(1.40290570022106,0.715991732016857,5.5845290818137));
#5256=CARTESIAN_POINT('Ctrl Pts',(1.39429976598019,0.725280259543278,5.57947689672541));
#5257=CARTESIAN_POINT('Ctrl Pts',(1.37429202304434,0.742032846767245,5.57390542856553));
#5258=CARTESIAN_POINT('Ctrl Pts',(1.36289688546797,0.749506871777696,5.57339216109808));
#5259=CARTESIAN_POINT('Ctrl Pts',(1.34084452821592,0.76116674603262,5.57643877096119));
#5260=CARTESIAN_POINT('Ctrl Pts',(1.32871459029889,0.766133383144486,5.58020335328619));
#5261=CARTESIAN_POINT('Ctrl Pts',(1.30571717897454,0.772681811266156,5.59204570008224));
#5262=CARTESIAN_POINT('Ctrl Pts',(1.29485633071097,0.77427304209217,5.60013110639566));
#5263=CARTESIAN_POINT('Ctrl Pts',(1.2770863685657,0.77427304209217,5.61790106854092));
#5264=CARTESIAN_POINT('Ctrl Pts',(1.26900096225229,0.772681811266156,5.6287619168045));
#5265=CARTESIAN_POINT('Ctrl Pts',(1.25715861545624,0.766133383144486,5.65175932812884));
#5266=CARTESIAN_POINT('Ctrl Pts',(1.25339403313124,0.76116674603262,5.66388926604588));
#5267=CARTESIAN_POINT('Ctrl Pts',(1.25034742326813,0.749506871777696,5.68594162329792));
#5268=CARTESIAN_POINT('Ctrl Pts',(1.25086069073558,0.742032846767245,5.69733676087429));
#5269=CARTESIAN_POINT('Ctrl Pts',(1.25643215889546,0.725280259543278,5.71734450381015));
#5270=CARTESIAN_POINT('Ctrl Pts',(1.26148434398375,0.715991732016857,5.72595043805101));
#5271=CARTESIAN_POINT('Ctrl Pts',(1.27404956194899,0.698221830356238,5.73851565601625));
#5272=CARTESIAN_POINT('Ctrl Pts',(1.28239441732645,0.688564081560337,5.74330676224113));
#5273=CARTESIAN_POINT('Ctrl Pts',(1.30145842274292,0.67047684793714,5.74793449288163));
#5274=CARTESIAN_POINT('Ctrl Pts',(1.31218429156503,0.662056333977536,5.74777849159482));
#5275=CARTESIAN_POINT('Ctrl Pts',(1.33297855127604,0.648617241117307,5.74347378419068));
#5276=CARTESIAN_POINT('Ctrl Pts',(1.34443775417856,0.642702041451141,5.73903846685116));
#5277=CARTESIAN_POINT('Ctrl Pts',(1.3664880711697,0.63481421967861,5.72624902572191));
#5278=CARTESIAN_POINT('Ctrl Pts',(1.3770863685657,0.63285168585486,5.71790106854092));
#5279=CARTESIAN_POINT('Ctrl Pts',(1.38597134963833,0.63285168585486,5.70901608746829));
#5280=CARTESIAN_POINT('',(1.45918830920368,0.777817459305203,5.64081169079632));
#5281=CARTESIAN_POINT('',(0.309188309203679,-0.848528137423857,4.49081169079632));
#5282=CARTESIAN_POINT('',(1.43620018859019,0.703885991122829,5.75924492642014));
#5283=CARTESIAN_POINT('Ctrl Pts',(1.43620018859019,0.703885991122829,5.75924492642014));
#5284=CARTESIAN_POINT('Ctrl Pts',(1.42731632321618,0.703885991122829,5.76812879179415));
#5285=CARTESIAN_POINT('Ctrl Pts',(1.41670673551834,0.705831016678426,5.77646450897213));
#5286=CARTESIAN_POINT('Ctrl Pts',(1.39461294702236,0.713657162034741,5.78921110107552));
#5287=CARTESIAN_POINT('Ctrl Pts',(1.38312226363248,0.719529169803534,5.79361633118594));
#5288=CARTESIAN_POINT('Ctrl Pts',(1.36226862086218,0.732888284319023,5.7978639998382));
#5289=CARTESIAN_POINT('Ctrl Pts',(1.35151161561087,0.741266387103756,5.7979891970858));
#5290=CARTESIAN_POINT('Ctrl Pts',(1.33240475326106,0.759293157295718,5.79331796315392));
#5291=CARTESIAN_POINT('Ctrl Pts',(1.32404877983516,0.768933614550882,5.78851487390242));
#5292=CARTESIAN_POINT('Ctrl Pts',(1.31148512609758,0.786701304059523,5.77595122016484));
#5293=CARTESIAN_POINT('Ctrl Pts',(1.30644473548592,0.796006166512776,5.76735794537877));
#5294=CARTESIAN_POINT('Ctrl Pts',(1.30091569824925,0.812819819637263,5.74739327972419));
#5295=CARTESIAN_POINT('Ctrl Pts',(1.30043258620615,0.820337643172962,5.73602796518216));
#5296=CARTESIAN_POINT('Ctrl Pts',(1.30353692145288,0.832079840080031,5.71403098900633));
#5297=CARTESIAN_POINT('Ctrl Pts',(1.30733274169053,0.837090012141718,5.70193089574369));
#5298=CARTESIAN_POINT('Ctrl Pts',(1.31921901153821,0.843699478096003,5.67897678499201));
#5299=CARTESIAN_POINT('Ctrl Pts',(1.32731632321618,0.845307347360138,5.66812879179415));
#5300=CARTESIAN_POINT('Ctrl Pts',(1.3450840539642,0.845307347360138,5.65036106104614));
#5301=CARTESIAN_POINT('Ctrl Pts',(1.35593204716206,0.843699478096003,5.64226374936816));
#5302=CARTESIAN_POINT('Ctrl Pts',(1.37888615791374,0.837090012141717,5.63037747952049));
#5303=CARTESIAN_POINT('Ctrl Pts',(1.39098625117638,0.832079840080031,5.62658165928283));
#5304=CARTESIAN_POINT('Ctrl Pts',(1.41298322735221,0.820337643172961,5.6234773240361));
#5305=CARTESIAN_POINT('Ctrl Pts',(1.42434854189423,0.812819819637263,5.6239604360792));
#5306=CARTESIAN_POINT('Ctrl Pts',(1.44431320754882,0.796006166512776,5.62948947331587));
#5307=CARTESIAN_POINT('Ctrl Pts',(1.45290648233489,0.786701304059524,5.63452986392753));
#5308=CARTESIAN_POINT('Ctrl Pts',(1.45918830920368,0.777817459305203,5.64081169079632));
#5309=CARTESIAN_POINT('Ctrl Pts',(1.45918830920368,0.777817459305203,5.64081169079632));
#5310=CARTESIAN_POINT('Ctrl Pts',(1.46547013607247,0.768933614550882,5.64709351766511));
#5311=CARTESIAN_POINT('Ctrl Pts',(1.47027322532397,0.759293157295718,5.65544949109102));
#5312=CARTESIAN_POINT('Ctrl Pts',(1.47494445925585,0.741266387103756,5.67455635344082));
#5313=CARTESIAN_POINT('Ctrl Pts',(1.47481926200825,0.732888284319023,5.68531335869214));
#5314=CARTESIAN_POINT('Ctrl Pts',(1.47057159335598,0.719529169803534,5.70616700146243));
#5315=CARTESIAN_POINT('Ctrl Pts',(1.46616636324556,0.713657162034742,5.71765768485231));
#5316=CARTESIAN_POINT('Ctrl Pts',(1.45341977114218,0.705831016678426,5.73975147334829));
#5317=CARTESIAN_POINT('Ctrl Pts',(1.4450840539642,0.703885991122829,5.75036106104614));
#5318=CARTESIAN_POINT('Ctrl Pts',(1.43620018859019,0.703885991122829,5.75924492642014));
#5319=CARTESIAN_POINT('Origin',(-0.327207793864214,-0.848528137423857,5.12720779386421));
#5320=CARTESIAN_POINT('',(-0.22493035136938,-0.845307347360138,5.22948523635905));
#5321=CARTESIAN_POINT('',(-0.206497115745559,-0.777817459305203,5.10649711574556));
#5322=CARTESIAN_POINT('Ctrl Pts',(-0.22493035136938,-0.845307347360138,
5.22948523635905));
#5323=CARTESIAN_POINT('Ctrl Pts',(-0.216046485995375,-0.845307347360138,
5.22060137098504));
#5324=CARTESIAN_POINT('Ctrl Pts',(-0.207949174317402,-0.843699478096003,
5.20975337778718));
#5325=CARTESIAN_POINT('Ctrl Pts',(-0.196062904469725,-0.837090012141717,
5.1867992670355));
#5326=CARTESIAN_POINT('Ctrl Pts',(-0.192267084232068,-0.832079840080031,
5.17469917377286));
#5327=CARTESIAN_POINT('Ctrl Pts',(-0.189162748985339,-0.820337643172961,
5.15270219759703));
#5328=CARTESIAN_POINT('Ctrl Pts',(-0.189645861028441,-0.812819819637263,
5.14133688305501));
#5329=CARTESIAN_POINT('Ctrl Pts',(-0.195174898265109,-0.796006166512776,
5.12137221740042));
#5330=CARTESIAN_POINT('Ctrl Pts',(-0.20021528887677,-0.786701304059523,
5.11277894261435));
#5331=CARTESIAN_POINT('Ctrl Pts',(-0.206497115745559,-0.777817459305202,
5.10649711574556));
#5332=CARTESIAN_POINT('Ctrl Pts',(-0.206497115745559,-0.777817459305202,
5.10649711574556));
#5333=CARTESIAN_POINT('Ctrl Pts',(-0.212778942614348,-0.768933614550881,
5.10021528887677));
#5334=CARTESIAN_POINT('Ctrl Pts',(-0.221134916040255,-0.759293157295718,
5.09541219962527));
#5335=CARTESIAN_POINT('Ctrl Pts',(-0.240241778390058,-0.741266387103756,
5.09074096569339));
#5336=CARTESIAN_POINT('Ctrl Pts',(-0.250998783641374,-0.732888284319023,
5.09086616294099));
#5337=CARTESIAN_POINT('Ctrl Pts',(-0.27185242641167,-0.719529169803534,
5.09511383159326));
#5338=CARTESIAN_POINT('Ctrl Pts',(-0.28334310980155,-0.713657162034742,
5.09951906170368));
#5339=CARTESIAN_POINT('Ctrl Pts',(-0.305436898297527,-0.705831016678426,
5.11226565380706));
#5340=CARTESIAN_POINT('Ctrl Pts',(-0.316046485995375,-0.703885991122829,
5.12060137098504));
#5341=CARTESIAN_POINT('Ctrl Pts',(-0.333814216743386,-0.703885991122829,
5.13836910173305));
#5342=CARTESIAN_POINT('Ctrl Pts',(-0.34214993392137,-0.705831016678427,
5.1489786894309));
#5343=CARTESIAN_POINT('Ctrl Pts',(-0.354896526024753,-0.713657162034741,
5.17107247792688));
#5344=CARTESIAN_POINT('Ctrl Pts',(-0.359301756135173,-0.719529169803534,
5.18256316131676));
#5345=CARTESIAN_POINT('Ctrl Pts',(-0.363549424787436,-0.732888284319023,
5.20341680408705));
#5346=CARTESIAN_POINT('Ctrl Pts',(-0.363674622035041,-0.741266387103756,
5.21417380933837));
#5347=CARTESIAN_POINT('Ctrl Pts',(-0.359003388103157,-0.759293157295718,
5.23328067168817));
#5348=CARTESIAN_POINT('Ctrl Pts',(-0.354200298851658,-0.768933614550882,
5.24163664511408));
#5349=CARTESIAN_POINT('Ctrl Pts',(-0.34163664511408,-0.786701304059523,
5.25420029885166));
#5350=CARTESIAN_POINT('Ctrl Pts',(-0.333043370328011,-0.796006166512776,
5.25924068946332));
#5351=CARTESIAN_POINT('Ctrl Pts',(-0.313078704673424,-0.812819819637263,
5.26476972669999));
#5352=CARTESIAN_POINT('Ctrl Pts',(-0.3017133901314,-0.820337643172961,5.26525283874309));
#5353=CARTESIAN_POINT('Ctrl Pts',(-0.279716413955571,-0.832079840080031,
5.26214850349636));
#5354=CARTESIAN_POINT('Ctrl Pts',(-0.267616320692928,-0.837090012141717,
5.2583526832587));
#5355=CARTESIAN_POINT('Ctrl Pts',(-0.244662209941247,-0.843699478096003,
5.24646641341103));
#5356=CARTESIAN_POINT('Ctrl Pts',(-0.233814216743386,-0.845307347360138,
5.23836910173305));
#5357=CARTESIAN_POINT('Ctrl Pts',(-0.22493035136938,-0.845307347360138,
5.22948523635905));
#5358=CARTESIAN_POINT('',(-0.156497115745559,-0.707106781186548,5.15649711574556));
#5359=CARTESIAN_POINT('',(-0.256497115745559,-0.848528137423857,5.05649711574556));
#5360=CARTESIAN_POINT('',(-0.174701512417524,-0.774273042092169,5.2797140753109));
#5361=CARTESIAN_POINT('Ctrl Pts',(-0.174701512417524,-0.774273042092169,
5.2797140753109));
#5362=CARTESIAN_POINT('Ctrl Pts',(-0.183586493490155,-0.774273042092169,
5.28859905638354));
#5363=CARTESIAN_POINT('Ctrl Pts',(-0.194447341753735,-0.772681811266156,
5.29668446269695));
#5364=CARTESIAN_POINT('Ctrl Pts',(-0.21744475307808,-0.766133383144486,
5.308526809493));
#5365=CARTESIAN_POINT('Ctrl Pts',(-0.229574690995115,-0.76116674603262,
5.312291391818));
#5366=CARTESIAN_POINT('Ctrl Pts',(-0.251627048247156,-0.749506871777696,
5.31533800168111));
#5367=CARTESIAN_POINT('Ctrl Pts',(-0.263022185823527,-0.742032846767245,
5.31482473421366));
#5368=CARTESIAN_POINT('Ctrl Pts',(-0.283029928759382,-0.725280259543278,
5.30925326605378));
#5369=CARTESIAN_POINT('Ctrl Pts',(-0.291635863000248,-0.715991732016857,
5.30420108096549));
#5370=CARTESIAN_POINT('Ctrl Pts',(-0.30420108096549,-0.698221830356238,
5.29163586300025));
#5371=CARTESIAN_POINT('Ctrl Pts',(-0.308992187190372,-0.688564081560337,
5.28329100762279));
#5372=CARTESIAN_POINT('Ctrl Pts',(-0.313619917830871,-0.67047684793714,
5.26422700220632));
#5373=CARTESIAN_POINT('Ctrl Pts',(-0.313463916544059,-0.662056333977536,
5.25350113338421));
#5374=CARTESIAN_POINT('Ctrl Pts',(-0.309159209139922,-0.648617241117307,
5.23270687367319));
#5375=CARTESIAN_POINT('Ctrl Pts',(-0.304723891800398,-0.642702041451141,
5.22124767077068));
#5376=CARTESIAN_POINT('Ctrl Pts',(-0.291934450671145,-0.63481421967861,
5.19919735377954));
#5377=CARTESIAN_POINT('Ctrl Pts',(-0.283586493490155,-0.63285168585486,
5.18859905638354));
#5378=CARTESIAN_POINT('Ctrl Pts',(-0.265816531344893,-0.63285168585486,
5.17082909423827));
#5379=CARTESIAN_POINT('Ctrl Pts',(-0.255218233948889,-0.634814219678611,
5.16248113705728));
#5380=CARTESIAN_POINT('Ctrl Pts',(-0.233167916957745,-0.642702041451141,
5.14969169592803));
#5381=CARTESIAN_POINT('Ctrl Pts',(-0.221708714055234,-0.648617241117307,
5.14525637858851));
#5382=CARTESIAN_POINT('Ctrl Pts',(-0.200914454344219,-0.662056333977536,
5.14095167118437));
#5383=CARTESIAN_POINT('Ctrl Pts',(-0.190188585522111,-0.67047684793714,
5.14079566989756));
#5384=CARTESIAN_POINT('Ctrl Pts',(-0.171124580105637,-0.688564081560337,
5.14542340053806));
#5385=CARTESIAN_POINT('Ctrl Pts',(-0.16277972472818,-0.698221830356238,
5.15021450676294));
#5386=CARTESIAN_POINT('Ctrl Pts',(-0.156497115745559,-0.707106781186548,
5.15649711574556));
#5387=CARTESIAN_POINT('Ctrl Pts',(-0.156497115745559,-0.707106781186547,
5.15649711574556));
#5388=CARTESIAN_POINT('Ctrl Pts',(-0.150214506762938,-0.715991732016857,
5.16277972472818));
#5389=CARTESIAN_POINT('Ctrl Pts',(-0.145162321674648,-0.725280259543278,
5.17138565896905));
#5390=CARTESIAN_POINT('Ctrl Pts',(-0.139590853514768,-0.742032846767245,
5.1913934019049));
#5391=CARTESIAN_POINT('Ctrl Pts',(-0.139077586047315,-0.749506871777696,
5.20278853948127));
#5392=CARTESIAN_POINT('Ctrl Pts',(-0.142124195910428,-0.76116674603262,
5.22484089673331));
#5393=CARTESIAN_POINT('Ctrl Pts',(-0.145888778235427,-0.766133383144486,
5.23697083465035));
#5394=CARTESIAN_POINT('Ctrl Pts',(-0.157731125031478,-0.772681811266156,
5.25996824597469));
#5395=CARTESIAN_POINT('Ctrl Pts',(-0.165816531344893,-0.774273042092169,
5.27082909423827));
#5396=CARTESIAN_POINT('Ctrl Pts',(-0.174701512417524,-0.774273042092169,
5.2797140753109));
#5397=CARTESIAN_POINT('Origin',(-0.327207793864214,-0.848528137423857,5.12720779386421));
#5398=CARTESIAN_POINT('',(0.820285924689096,0.63285168585486,6.27470151241752));
#5399=CARTESIAN_POINT('',(0.843502884254441,0.707106781186547,6.15649711574556));
#5400=CARTESIAN_POINT('Ctrl Pts',(0.820285924689096,0.63285168585486,6.27470151241752));
#5401=CARTESIAN_POINT('Ctrl Pts',(0.829170905761727,0.63285168585486,6.26581653134489));
#5402=CARTESIAN_POINT('Ctrl Pts',(0.837518862942717,0.634814219678611,6.25521823394889));
#5403=CARTESIAN_POINT('Ctrl Pts',(0.85030830407197,0.642702041451141,6.23316791695775));
#5404=CARTESIAN_POINT('Ctrl Pts',(0.854743621411493,0.648617241117307,6.22170871405523));
#5405=CARTESIAN_POINT('Ctrl Pts',(0.859048328815631,0.662056333977536,6.20091445434422));
#5406=CARTESIAN_POINT('Ctrl Pts',(0.859204330102443,0.67047684793714,6.19018858552211));
#5407=CARTESIAN_POINT('Ctrl Pts',(0.854576599461944,0.688564081560337,6.17112458010564));
#5408=CARTESIAN_POINT('Ctrl Pts',(0.849785493237061,0.698221830356238,6.16277972472818));
#5409=CARTESIAN_POINT('Ctrl Pts',(0.843502884254441,0.707106781186547,6.15649711574556));
#5410=CARTESIAN_POINT('Ctrl Pts',(0.843502884254441,0.707106781186548,6.15649711574556));
#5411=CARTESIAN_POINT('Ctrl Pts',(0.83722027527182,0.715991732016857,6.15021450676294));
#5412=CARTESIAN_POINT('Ctrl Pts',(0.828614341030954,0.725280259543277,6.14516232167465));
#5413=CARTESIAN_POINT('Ctrl Pts',(0.808606598095098,0.742032846767245,6.13959085351477));
#5414=CARTESIAN_POINT('Ctrl Pts',(0.797211460518727,0.749506871777696,6.13907758604732));
#5415=CARTESIAN_POINT('Ctrl Pts',(0.775159103266687,0.76116674603262,6.14212419591043));
#5416=CARTESIAN_POINT('Ctrl Pts',(0.763029165349651,0.766133383144486,6.14588877823543));
#5417=CARTESIAN_POINT('Ctrl Pts',(0.740031754025306,0.772681811266156,6.15773112503148));
#5418=CARTESIAN_POINT('Ctrl Pts',(0.729170905761727,0.77427304209217,6.16581653134489));
#5419=CARTESIAN_POINT('Ctrl Pts',(0.711400943616465,0.77427304209217,6.18358649349016));
#5420=CARTESIAN_POINT('Ctrl Pts',(0.703315537303049,0.772681811266156,6.19444734175373));
#5421=CARTESIAN_POINT('Ctrl Pts',(0.691473190506998,0.766133383144486,6.21744475307808));
#5422=CARTESIAN_POINT('Ctrl Pts',(0.687708608181999,0.76116674603262,6.22957469099512));
#5423=CARTESIAN_POINT('Ctrl Pts',(0.684661998318887,0.749506871777696,6.25162704824716));
#5424=CARTESIAN_POINT('Ctrl Pts',(0.685175265786339,0.742032846767245,6.26302218582353));
#5425=CARTESIAN_POINT('Ctrl Pts',(0.69074673394622,0.725280259543278,6.28302992875938));
#5426=CARTESIAN_POINT('Ctrl Pts',(0.69579891903451,0.715991732016857,6.29163586300025));
#5427=CARTESIAN_POINT('Ctrl Pts',(0.708364136999752,0.698221830356238,6.30420108096549));
#5428=CARTESIAN_POINT('Ctrl Pts',(0.716708992377209,0.688564081560337,6.30899218719037));
#5429=CARTESIAN_POINT('Ctrl Pts',(0.735772997793683,0.67047684793714,6.31361991783087));
#5430=CARTESIAN_POINT('Ctrl Pts',(0.74649886661579,0.662056333977536,6.31346391654406));
#5431=CARTESIAN_POINT('Ctrl Pts',(0.767293126326806,0.648617241117307,6.30915920913992));
#5432=CARTESIAN_POINT('Ctrl Pts',(0.778752329229317,0.642702041451141,6.3047238918004));
#5433=CARTESIAN_POINT('Ctrl Pts',(0.80080264622046,0.634814219678611,6.29193445067115));
#5434=CARTESIAN_POINT('Ctrl Pts',(0.811400943616465,0.63285168585486,6.28358649349016));
#5435=CARTESIAN_POINT('Ctrl Pts',(0.820285924689096,0.63285168585486,6.27470151241752));
#5436=CARTESIAN_POINT('',(0.893502884254441,0.777817459305203,6.20649711574556));
#5437=CARTESIAN_POINT('',(-0.256497115745559,-0.848528137423857,5.05649711574556));
#5438=CARTESIAN_POINT('',(0.870514763640952,0.703885991122829,6.32493035136938));
#5439=CARTESIAN_POINT('Ctrl Pts',(0.870514763640951,0.703885991122829,6.32493035136938));
#5440=CARTESIAN_POINT('Ctrl Pts',(0.861630898266946,0.703885991122829,6.33381421674339));
#5441=CARTESIAN_POINT('Ctrl Pts',(0.851021310569098,0.705831016678427,6.34214993392137));
#5442=CARTESIAN_POINT('Ctrl Pts',(0.828927522073122,0.713657162034742,6.35489652602475));
#5443=CARTESIAN_POINT('Ctrl Pts',(0.817436838683242,0.719529169803534,6.35930175613517));
#5444=CARTESIAN_POINT('Ctrl Pts',(0.796583195912946,0.732888284319023,6.36354942478744));
#5445=CARTESIAN_POINT('Ctrl Pts',(0.785826190661629,0.741266387103756,6.36367462203504));
#5446=CARTESIAN_POINT('Ctrl Pts',(0.766719328311827,0.759293157295718,6.35900338810316));
#5447=CARTESIAN_POINT('Ctrl Pts',(0.75836335488592,0.768933614550882,6.35420029885166));
#5448=CARTESIAN_POINT('Ctrl Pts',(0.745799701148342,0.786701304059523,6.34163664511408));
#5449=CARTESIAN_POINT('Ctrl Pts',(0.740759310536681,0.796006166512776,6.33304337032801));
#5450=CARTESIAN_POINT('Ctrl Pts',(0.735230273300012,0.812819819637263,6.31307870467342));
#5451=CARTESIAN_POINT('Ctrl Pts',(0.73474716125691,0.820337643172962,6.3017133901314));
#5452=CARTESIAN_POINT('Ctrl Pts',(0.73785149650364,0.832079840080031,6.27971641395557));
#5453=CARTESIAN_POINT('Ctrl Pts',(0.741647316741297,0.837090012141717,6.26761632069293));
#5454=CARTESIAN_POINT('Ctrl Pts',(0.753533586588974,0.843699478096003,6.24466220994125));
#5455=CARTESIAN_POINT('Ctrl Pts',(0.761630898266946,0.845307347360138,6.23381421674339));
#5456=CARTESIAN_POINT('Ctrl Pts',(0.779398629014958,0.845307347360138,6.21604648599538));
#5457=CARTESIAN_POINT('Ctrl Pts',(0.790246622212818,0.843699478096003,6.2079491743174));
#5458=CARTESIAN_POINT('Ctrl Pts',(0.8132007329645,0.837090012141717,6.19606290446973));
#5459=CARTESIAN_POINT('Ctrl Pts',(0.825300826227143,0.832079840080031,6.19226708423207));
#5460=CARTESIAN_POINT('Ctrl Pts',(0.847297802402972,0.820337643172961,6.18916274898534));
#5461=CARTESIAN_POINT('Ctrl Pts',(0.858663116944995,0.812819819637263,6.18964586102844));
#5462=CARTESIAN_POINT('Ctrl Pts',(0.878627782599582,0.796006166512776,6.19517489826511));
#5463=CARTESIAN_POINT('Ctrl Pts',(0.887221057385652,0.786701304059524,6.20021528887677));
#5464=CARTESIAN_POINT('Ctrl Pts',(0.893502884254441,0.777817459305203,6.20649711574556));
#5465=CARTESIAN_POINT('Ctrl Pts',(0.893502884254441,0.777817459305203,6.20649711574556));
#5466=CARTESIAN_POINT('Ctrl Pts',(0.89978471112323,0.768933614550882,6.21277894261435));
#5467=CARTESIAN_POINT('Ctrl Pts',(0.904587800374729,0.759293157295718,6.22113491604026));
#5468=CARTESIAN_POINT('Ctrl Pts',(0.909259034306612,0.741266387103756,6.24024177839006));
#5469=CARTESIAN_POINT('Ctrl Pts',(0.909133837059008,0.732888284319023,6.25099878364137));
#5470=CARTESIAN_POINT('Ctrl Pts',(0.904886168406745,0.719529169803534,6.27185242641167));
#5471=CARTESIAN_POINT('Ctrl Pts',(0.900480938296325,0.713657162034741,6.28334310980155));
#5472=CARTESIAN_POINT('Ctrl Pts',(0.887734346192942,0.705831016678426,6.30543689829753));
#5473=CARTESIAN_POINT('Ctrl Pts',(0.879398629014957,0.703885991122829,6.31604648599538));
#5474=CARTESIAN_POINT('Ctrl Pts',(0.870514763640952,0.703885991122829,6.32493035136938));
#5475=CARTESIAN_POINT('Origin',(1.93553390593274,-0.848528137423857,2.86446609406726));
#5476=CARTESIAN_POINT('',(2.03781134842757,-0.845307347360138,2.9667435365621));
#5477=CARTESIAN_POINT('',(2.05624458405139,-0.777817459305203,2.84375541594861));
#5478=CARTESIAN_POINT('Ctrl Pts',(2.03781134842757,-0.845307347360138,2.9667435365621));
#5479=CARTESIAN_POINT('Ctrl Pts',(2.04669521380158,-0.845307347360138,2.95785967118809));
#5480=CARTESIAN_POINT('Ctrl Pts',(2.05479252547955,-0.843699478096003,2.94701167799023));
#5481=CARTESIAN_POINT('Ctrl Pts',(2.06667879532723,-0.837090012141717,2.92405756723855));
#5482=CARTESIAN_POINT('Ctrl Pts',(2.07047461556488,-0.832079840080031,2.9119574739759));
#5483=CARTESIAN_POINT('Ctrl Pts',(2.07357895081161,-0.820337643172961,2.88996049780008));
#5484=CARTESIAN_POINT('Ctrl Pts',(2.07309583876851,-0.812819819637263,2.87859518325805));
#5485=CARTESIAN_POINT('Ctrl Pts',(2.06756680153184,-0.796006166512776,2.85863051760347));
#5486=CARTESIAN_POINT('Ctrl Pts',(2.06252641092018,-0.786701304059523,2.8500372428174));
#5487=CARTESIAN_POINT('Ctrl Pts',(2.05624458405139,-0.777817459305202,2.84375541594861));
#5488=CARTESIAN_POINT('Ctrl Pts',(2.05624458405139,-0.777817459305202,2.84375541594861));
#5489=CARTESIAN_POINT('Ctrl Pts',(2.0499627571826,-0.768933614550881,2.83747358907982));
#5490=CARTESIAN_POINT('Ctrl Pts',(2.0416067837567,-0.759293157295718,2.83267049982832));
#5491=CARTESIAN_POINT('Ctrl Pts',(2.0224999214069,-0.741266387103757,2.82799926589644));
#5492=CARTESIAN_POINT('Ctrl Pts',(2.01174291615558,-0.732888284319023,2.82812446314404));
#5493=CARTESIAN_POINT('Ctrl Pts',(1.99088927338528,-0.719529169803534,2.8323721317963));
#5494=CARTESIAN_POINT('Ctrl Pts',(1.9793985899954,-0.713657162034742,2.83677736190672));
#5495=CARTESIAN_POINT('Ctrl Pts',(1.95730480149943,-0.705831016678427,2.84952395401011));
#5496=CARTESIAN_POINT('Ctrl Pts',(1.94669521380158,-0.703885991122829,2.85785967118809));
#5497=CARTESIAN_POINT('Ctrl Pts',(1.92892748305357,-0.703885991122829,2.8756274019361));
#5498=CARTESIAN_POINT('Ctrl Pts',(1.92059176587558,-0.705831016678427,2.88623698963395));
#5499=CARTESIAN_POINT('Ctrl Pts',(1.9078451737722,-0.713657162034742,2.90833077812993));
#5500=CARTESIAN_POINT('Ctrl Pts',(1.90343994366178,-0.719529169803534,2.91982146151981));
#5501=CARTESIAN_POINT('Ctrl Pts',(1.89919227500952,-0.732888284319023,2.9406751042901));
#5502=CARTESIAN_POINT('Ctrl Pts',(1.89906707776191,-0.741266387103756,2.95143210954142));
#5503=CARTESIAN_POINT('Ctrl Pts',(1.9037383116938,-0.759293157295718,2.97053897189122));
#5504=CARTESIAN_POINT('Ctrl Pts',(1.9085414009453,-0.768933614550882,2.97889494531713));
#5505=CARTESIAN_POINT('Ctrl Pts',(1.92110505468287,-0.786701304059523,2.99145859905471));
#5506=CARTESIAN_POINT('Ctrl Pts',(1.92969832946894,-0.796006166512775,2.99649898966637));
#5507=CARTESIAN_POINT('Ctrl Pts',(1.94966299512353,-0.812819819637263,3.00202802690304));
#5508=CARTESIAN_POINT('Ctrl Pts',(1.96102830966555,-0.820337643172961,3.00251113894614));
#5509=CARTESIAN_POINT('Ctrl Pts',(1.98302528584138,-0.832079840080031,2.99940680369941));
#5510=CARTESIAN_POINT('Ctrl Pts',(1.99512537910402,-0.837090012141717,2.99561098346175));
#5511=CARTESIAN_POINT('Ctrl Pts',(2.01807948985571,-0.843699478096003,2.98372471361407));
#5512=CARTESIAN_POINT('Ctrl Pts',(2.02892748305357,-0.845307347360138,2.9756274019361));
#5513=CARTESIAN_POINT('Ctrl Pts',(2.03781134842757,-0.845307347360138,2.9667435365621));
#5514=CARTESIAN_POINT('',(2.10624458405139,-0.707106781186548,2.89375541594861));
#5515=CARTESIAN_POINT('',(2.00624458405139,-0.848528137423857,2.79375541594861));
#5516=CARTESIAN_POINT('',(2.08804018737943,-0.774273042092169,3.01697237551395));
#5517=CARTESIAN_POINT('Ctrl Pts',(2.08804018737943,-0.774273042092169,3.01697237551395));
#5518=CARTESIAN_POINT('Ctrl Pts',(2.0791552063068,-0.774273042092169,3.02585735658658));
#5519=CARTESIAN_POINT('Ctrl Pts',(2.06829435804322,-0.772681811266156,3.0339427629));
#5520=CARTESIAN_POINT('Ctrl Pts',(2.04529694671887,-0.766133383144485,3.04578510969605));
#5521=CARTESIAN_POINT('Ctrl Pts',(2.03316700880184,-0.761166746032619,3.04954969202105));
#5522=CARTESIAN_POINT('Ctrl Pts',(2.0111146515498,-0.749506871777695,3.05259630188416));
#5523=CARTESIAN_POINT('Ctrl Pts',(1.99971951397343,-0.742032846767244,3.05208303441671));
#5524=CARTESIAN_POINT('Ctrl Pts',(1.97971177103757,-0.725280259543277,3.04651156625683));
#5525=CARTESIAN_POINT('Ctrl Pts',(1.9711058367967,-0.715991732016857,3.04145938116854));
#5526=CARTESIAN_POINT('Ctrl Pts',(1.95854061883146,-0.698221830356238,3.0288941632033));
#5527=CARTESIAN_POINT('Ctrl Pts',(1.95374951260658,-0.688564081560337,3.02054930782584));
#5528=CARTESIAN_POINT('Ctrl Pts',(1.94912178196608,-0.67047684793714,3.00148530240937));
#5529=CARTESIAN_POINT('Ctrl Pts',(1.94927778325289,-0.662056333977536,2.99075943358726));
#5530=CARTESIAN_POINT('Ctrl Pts',(1.95358249065703,-0.648617241117307,2.96996517387624));
#5531=CARTESIAN_POINT('Ctrl Pts',(1.95801780799656,-0.642702041451141,2.95850597097373));
#5532=CARTESIAN_POINT('Ctrl Pts',(1.97080724912581,-0.634814219678611,2.93645565398259));
#5533=CARTESIAN_POINT('Ctrl Pts',(1.9791552063068,-0.63285168585486,2.92585735658658));
#5534=CARTESIAN_POINT('Ctrl Pts',(1.99692516845206,-0.63285168585486,2.90808739444132));
#5535=CARTESIAN_POINT('Ctrl Pts',(2.00752346584806,-0.634814219678611,2.89973943726033));
#5536=CARTESIAN_POINT('Ctrl Pts',(2.02957378283921,-0.642702041451141,2.88694999613108));
#5537=CARTESIAN_POINT('Ctrl Pts',(2.04103298574172,-0.648617241117307,2.88251467879155));
#5538=CARTESIAN_POINT('Ctrl Pts',(2.06182724545273,-0.662056333977536,2.87820997138742));
#5539=CARTESIAN_POINT('Ctrl Pts',(2.07255311427484,-0.67047684793714,2.87805397010061));
#5540=CARTESIAN_POINT('Ctrl Pts',(2.09161711969131,-0.688564081560337,2.8826817007411));
#5541=CARTESIAN_POINT('Ctrl Pts',(2.09996197506877,-0.698221830356238,2.88747280696599));
#5542=CARTESIAN_POINT('Ctrl Pts',(2.10624458405139,-0.707106781186548,2.89375541594861));
#5543=CARTESIAN_POINT('Ctrl Pts',(2.10624458405139,-0.707106781186548,2.89375541594861));
#5544=CARTESIAN_POINT('Ctrl Pts',(2.11252719303401,-0.715991732016857,2.90003802493123));
#5545=CARTESIAN_POINT('Ctrl Pts',(2.1175793781223,-0.725280259543277,2.90864395917209));
#5546=CARTESIAN_POINT('Ctrl Pts',(2.12315084628218,-0.742032846767244,2.92865170210795));
#5547=CARTESIAN_POINT('Ctrl Pts',(2.12366411374964,-0.749506871777695,2.94004683968432));
#5548=CARTESIAN_POINT('Ctrl Pts',(2.12061750388653,-0.761166746032619,2.96209919693636));
#5549=CARTESIAN_POINT('Ctrl Pts',(2.11685292156153,-0.766133383144485,2.9742291348534));
#5550=CARTESIAN_POINT('Ctrl Pts',(2.10501057476547,-0.772681811266156,2.99722654617774));
#5551=CARTESIAN_POINT('Ctrl Pts',(2.09692516845206,-0.774273042092169,3.00808739444132));
#5552=CARTESIAN_POINT('Ctrl Pts',(2.08804018737943,-0.774273042092169,3.01697237551395));
#5553=CARTESIAN_POINT('Origin',(1.93553390593274,-0.848528137423857,2.86446609406726));
#5554=CARTESIAN_POINT('',(3.08302762448605,0.63285168585486,4.01195981262057));
#5555=CARTESIAN_POINT('',(3.10624458405139,0.707106781186548,3.89375541594861));
#5556=CARTESIAN_POINT('Ctrl Pts',(3.08302762448605,0.63285168585486,4.01195981262057));
#5557=CARTESIAN_POINT('Ctrl Pts',(3.09191260555868,0.63285168585486,4.00307483154794));
#5558=CARTESIAN_POINT('Ctrl Pts',(3.10026056273967,0.634814219678611,3.99247653415194));
#5559=CARTESIAN_POINT('Ctrl Pts',(3.11305000386892,0.642702041451141,3.97042621716079));
#5560=CARTESIAN_POINT('Ctrl Pts',(3.11748532120845,0.648617241117307,3.95896701425828));
#5561=CARTESIAN_POINT('Ctrl Pts',(3.12179002861258,0.662056333977536,3.93817275454727));
#5562=CARTESIAN_POINT('Ctrl Pts',(3.1219460298994,0.67047684793714,3.92744688572516));
#5563=CARTESIAN_POINT('Ctrl Pts',(3.1173182992589,0.688564081560338,3.90838288030869));
#5564=CARTESIAN_POINT('Ctrl Pts',(3.11252719303401,0.698221830356238,3.90003802493123));
#5565=CARTESIAN_POINT('Ctrl Pts',(3.10624458405139,0.707106781186548,3.89375541594861));
#5566=CARTESIAN_POINT('Ctrl Pts',(3.10624458405139,0.707106781186548,3.89375541594861));
#5567=CARTESIAN_POINT('Ctrl Pts',(3.09996197506877,0.715991732016857,3.88747280696599));
#5568=CARTESIAN_POINT('Ctrl Pts',(3.09135604082791,0.725280259543277,3.8824206218777));
#5569=CARTESIAN_POINT('Ctrl Pts',(3.07134829789205,0.742032846767244,3.87684915371782));
#5570=CARTESIAN_POINT('Ctrl Pts',(3.05995316031568,0.749506871777695,3.87633588625036));
#5571=CARTESIAN_POINT('Ctrl Pts',(3.03790080306364,0.761166746032619,3.87938249611348));
#5572=CARTESIAN_POINT('Ctrl Pts',(3.02577086514661,0.766133383144485,3.88314707843847));
#5573=CARTESIAN_POINT('Ctrl Pts',(3.00277345382226,0.772681811266156,3.89498942523453));
#5574=CARTESIAN_POINT('Ctrl Pts',(2.99191260555868,0.774273042092169,3.90307483154794));
#5575=CARTESIAN_POINT('Ctrl Pts',(2.97414264341342,0.774273042092169,3.9208447936932));
#5576=CARTESIAN_POINT('Ctrl Pts',(2.9660572371,0.772681811266156,3.93170564195678));
#5577=CARTESIAN_POINT('Ctrl Pts',(2.95421489030395,0.766133383144486,3.95470305328113));
#5578=CARTESIAN_POINT('Ctrl Pts',(2.95045030797895,0.761166746032619,3.96683299119816));
#5579=CARTESIAN_POINT('Ctrl Pts',(2.94740369811584,0.749506871777695,3.9888853484502));
#5580=CARTESIAN_POINT('Ctrl Pts',(2.94791696558329,0.742032846767244,4.00028048602658));
#5581=CARTESIAN_POINT('Ctrl Pts',(2.95348843374317,0.725280259543277,4.02028822896243));
#5582=CARTESIAN_POINT('Ctrl Pts',(2.95854061883146,0.715991732016857,4.0288941632033));
#5583=CARTESIAN_POINT('Ctrl Pts',(2.9711058367967,0.698221830356238,4.04145938116854));
#5584=CARTESIAN_POINT('Ctrl Pts',(2.97945069217416,0.688564081560338,4.04625048739342));
#5585=CARTESIAN_POINT('Ctrl Pts',(2.99851469759064,0.67047684793714,4.05087821803392));
#5586=CARTESIAN_POINT('Ctrl Pts',(3.00924056641274,0.662056333977536,4.05072221674711));
#5587=CARTESIAN_POINT('Ctrl Pts',(3.03003482612376,0.648617241117307,4.04641750934297));
#5588=CARTESIAN_POINT('Ctrl Pts',(3.04149402902627,0.642702041451142,4.04198219200345));
#5589=CARTESIAN_POINT('Ctrl Pts',(3.06354434601741,0.634814219678611,4.02919275087419));
#5590=CARTESIAN_POINT('Ctrl Pts',(3.07414264341342,0.63285168585486,4.0208447936932));
#5591=CARTESIAN_POINT('Ctrl Pts',(3.08302762448605,0.63285168585486,4.01195981262057));
#5592=CARTESIAN_POINT('',(3.15624458405139,0.777817459305203,3.94375541594861));
#5593=CARTESIAN_POINT('',(2.00624458405139,-0.848528137423857,2.79375541594861));
#5594=CARTESIAN_POINT('',(3.1332564634379,0.703885991122829,4.06218865157243));
#5595=CARTESIAN_POINT('Ctrl Pts',(3.1332564634379,0.703885991122829,4.06218865157243));
#5596=CARTESIAN_POINT('Ctrl Pts',(3.1243725980639,0.703885991122829,4.07107251694644));
#5597=CARTESIAN_POINT('Ctrl Pts',(3.11376301036605,0.705831016678427,4.07940823412442));
#5598=CARTESIAN_POINT('Ctrl Pts',(3.09166922187007,0.713657162034742,4.0921548262278));
#5599=CARTESIAN_POINT('Ctrl Pts',(3.08017853848019,0.719529169803534,4.09656005633822));
#5600=CARTESIAN_POINT('Ctrl Pts',(3.0593248957099,0.732888284319023,4.10080772499048));
#5601=CARTESIAN_POINT('Ctrl Pts',(3.04856789045858,0.741266387103756,4.10093292223809));
#5602=CARTESIAN_POINT('Ctrl Pts',(3.02946102810878,0.759293157295718,4.09626168830621));
#5603=CARTESIAN_POINT('Ctrl Pts',(3.02110505468287,0.768933614550882,4.09145859905471));
#5604=CARTESIAN_POINT('Ctrl Pts',(3.00854140094529,0.786701304059523,4.07889494531713));
#5605=CARTESIAN_POINT('Ctrl Pts',(3.00350101033363,0.796006166512776,4.07030167053106));
#5606=CARTESIAN_POINT('Ctrl Pts',(2.99797197309697,0.812819819637263,4.05033700487647));
#5607=CARTESIAN_POINT('Ctrl Pts',(2.99748886105386,0.820337643172961,4.03897169033445));
#5608=CARTESIAN_POINT('Ctrl Pts',(3.00059319630059,0.832079840080031,4.01697471415862));
#5609=CARTESIAN_POINT('Ctrl Pts',(3.00438901653825,0.837090012141717,4.00487462089598));
#5610=CARTESIAN_POINT('Ctrl Pts',(3.01627528638593,0.843699478096003,3.9819205101443));
#5611=CARTESIAN_POINT('Ctrl Pts',(3.0243725980639,0.845307347360138,3.97107251694643));
#5612=CARTESIAN_POINT('Ctrl Pts',(3.04214032881191,0.845307347360138,3.95330478619842));
#5613=CARTESIAN_POINT('Ctrl Pts',(3.05298832200977,0.843699478096002,3.94520747452045));
#5614=CARTESIAN_POINT('Ctrl Pts',(3.07594243276145,0.837090012141716,3.93332120467277));
#5615=CARTESIAN_POINT('Ctrl Pts',(3.0880425260241,0.832079840080031,3.92952538443512));
#5616=CARTESIAN_POINT('Ctrl Pts',(3.11003950219992,0.820337643172961,3.92642104918839));
#5617=CARTESIAN_POINT('Ctrl Pts',(3.12140481674195,0.812819819637263,3.92690416123149));
#5618=CARTESIAN_POINT('Ctrl Pts',(3.14136948239654,0.796006166512776,3.93243319846816));
#5619=CARTESIAN_POINT('Ctrl Pts',(3.1499627571826,0.786701304059523,3.93747358907982));
#5620=CARTESIAN_POINT('Ctrl Pts',(3.15624458405139,0.777817459305203,3.94375541594861));
#5621=CARTESIAN_POINT('Ctrl Pts',(3.15624458405139,0.777817459305203,3.94375541594861));
#5622=CARTESIAN_POINT('Ctrl Pts',(3.16252641092018,0.768933614550882,3.9500372428174));
#5623=CARTESIAN_POINT('Ctrl Pts',(3.16732950017168,0.759293157295718,3.9583932162433));
#5624=CARTESIAN_POINT('Ctrl Pts',(3.17200073410356,0.741266387103756,3.97750007859311));
#5625=CARTESIAN_POINT('Ctrl Pts',(3.17187553685596,0.732888284319023,3.98825708384442));
#5626=CARTESIAN_POINT('Ctrl Pts',(3.1676278682037,0.719529169803534,4.00911072661472));
#5627=CARTESIAN_POINT('Ctrl Pts',(3.16322263809328,0.713657162034742,4.0206014100046));
#5628=CARTESIAN_POINT('Ctrl Pts',(3.1504760459899,0.705831016678427,4.04269519850057));
#5629=CARTESIAN_POINT('Ctrl Pts',(3.14214032881191,0.703885991122829,4.05330478619842));
#5630=CARTESIAN_POINT('Ctrl Pts',(3.1332564634379,0.703885991122829,4.06218865157243));
#5631=CARTESIAN_POINT('Origin',(3.10121933088198,-1.2,2.89878066911802));
#5632=CARTESIAN_POINT('',(3.17193000900063,-1.09544511501033,2.96949134723668));
#5633=CARTESIAN_POINT('',(3.17193000900063,-1.1,2.82806999099937));
#5634=CARTESIAN_POINT('Ctrl Pts',(3.17193000900063,-1.09544511501033,2.96949134723668));
#5635=CARTESIAN_POINT('Ctrl Pts',(3.18081387437464,-1.09544511501033,2.96060748186267));
#5636=CARTESIAN_POINT('Ctrl Pts',(3.18851007940269,-1.09568352051035,2.94935838201489));
#5637=CARTESIAN_POINT('Ctrl Pts',(3.19871246404707,-1.09654384276605,2.92472038605991));
#5638=CARTESIAN_POINT('Ctrl Pts',(3.20121933088198,-1.09715325263881,2.91133133939452));
#5639=CARTESIAN_POINT('Ctrl Pts',(3.20121933088198,-1.09829658604435,2.88623002797196));
#5640=CARTESIAN_POINT('Ctrl Pts',(3.19871246897122,-1.09890489533505,2.87284096356229));
#5641=CARTESIAN_POINT('Ctrl Pts',(3.18851007152196,-1.09976269863984,2.8482029376951));
#5642=CARTESIAN_POINT('Ctrl Pts',(3.18081385375495,-1.1,2.83695383575369));
#5643=CARTESIAN_POINT('Ctrl Pts',(3.17193000900063,-1.1,2.82806999099937));
#5644=CARTESIAN_POINT('Ctrl Pts',(3.17193000900063,-1.1,2.82806999099937));
#5645=CARTESIAN_POINT('Ctrl Pts',(3.16304616424631,-1.1,2.81918614624505));
#5646=CARTESIAN_POINT('Ctrl Pts',(3.1517970623049,-1.09976269863984,2.81148992847805));
#5647=CARTESIAN_POINT('Ctrl Pts',(3.12715903643772,-1.09890489533505,2.80128753102878));
#5648=CARTESIAN_POINT('Ctrl Pts',(3.11376997202804,-1.09829658604435,2.79878066911802));
#5649=CARTESIAN_POINT('Ctrl Pts',(3.08866866060548,-1.09715325263881,2.79878066911802));
#5650=CARTESIAN_POINT('Ctrl Pts',(3.07527961394009,-1.09654384276605,2.80128753595294));
#5651=CARTESIAN_POINT('Ctrl Pts',(3.05064161798511,-1.09568352051035,2.81148992059731));
#5652=CARTESIAN_POINT('Ctrl Pts',(3.03939251813733,-1.09544511501033,2.81918612562536));
#5653=CARTESIAN_POINT('Ctrl Pts',(3.02162478738932,-1.09544511501033,2.83695385637338));
#5654=CARTESIAN_POINT('Ctrl Pts',(3.01392858236127,-1.09568352051035,2.84820295622116));
#5655=CARTESIAN_POINT('Ctrl Pts',(3.00372619771689,-1.09654384276605,2.87284095217614));
#5656=CARTESIAN_POINT('Ctrl Pts',(3.00121933088198,-1.09715325263881,2.88622999884153));
#5657=CARTESIAN_POINT('Ctrl Pts',(3.00121933088198,-1.09829658604435,2.91133131026409));
#5658=CARTESIAN_POINT('Ctrl Pts',(3.00372619279273,-1.09890489533505,2.92472037467376));
#5659=CARTESIAN_POINT('Ctrl Pts',(3.013928590242,-1.09976269863984,2.94935840054095));
#5660=CARTESIAN_POINT('Ctrl Pts',(3.021624808009,-1.1,2.96060750248236));
#5661=CARTESIAN_POINT('Ctrl Pts',(3.03939249751764,-1.1,2.978375191991));
#5662=CARTESIAN_POINT('Ctrl Pts',(3.05064159945906,-1.09976269863984,2.986071409758));
#5663=CARTESIAN_POINT('Ctrl Pts',(3.07527962532624,-1.09890489533505,2.99627380720727));
#5664=CARTESIAN_POINT('Ctrl Pts',(3.08866868973591,-1.09829658604435,2.99878066911802));
#5665=CARTESIAN_POINT('Ctrl Pts',(3.11377000115847,-1.09715325263881,2.99878066911802));
#5666=CARTESIAN_POINT('Ctrl Pts',(3.12715904782386,-1.09654384276605,2.99627380228311));
#5667=CARTESIAN_POINT('Ctrl Pts',(3.15179704377884,-1.09568352051035,2.98607141763874));
#5668=CARTESIAN_POINT('Ctrl Pts',(3.16304614362662,-1.09544511501033,2.97837521261068));
#5669=CARTESIAN_POINT('Ctrl Pts',(3.17193000900063,-1.09544511501033,2.96949134723668));
#5670=CARTESIAN_POINT('',(3.17193000900063,-1.,2.82806999099937));
#5671=CARTESIAN_POINT('',(3.17193000900063,-1.2,2.82806999099937));
#5672=CARTESIAN_POINT('',(3.17193000900063,-0.99498743710662,2.96949134723668));
#5673=CARTESIAN_POINT('Ctrl Pts',(3.17193000900063,-0.99498743710662,2.96949134723668));
#5674=CARTESIAN_POINT('Ctrl Pts',(3.163045027928,-0.99498743710662,2.97837632830931));
#5675=CARTESIAN_POINT('Ctrl Pts',(3.15179501831462,-0.995249987974195,2.98607257327293));
#5676=CARTESIAN_POINT('Ctrl Pts',(3.12715701430732,-0.996197082307396,2.99627432738602));
#5677=CARTESIAN_POINT('Ctrl Pts',(3.11376883579729,-0.996867817321921,2.99878066911802));
#5678=CARTESIAN_POINT('Ctrl Pts',(3.08866986868214,-0.998125914862946,2.99878066911802));
#5679=CARTESIAN_POINT('Ctrl Pts',(3.07528166414265,-0.99879518361721,2.99627433468746));
#5680=CARTESIAN_POINT('Ctrl Pts',(3.05064361633108,-0.999738921136592,2.98607256165186));
#5681=CARTESIAN_POINT('Ctrl Pts',(3.03939360359363,-1.,2.97837629806699));
#5682=CARTESIAN_POINT('Ctrl Pts',(3.02162370193301,-1.,2.96060639640637));
#5683=CARTESIAN_POINT('Ctrl Pts',(3.01392743834814,-0.999738921136592,2.94935638366892));
#5684=CARTESIAN_POINT('Ctrl Pts',(3.00372566531254,-0.99879518361721,2.92471833585735));
#5685=CARTESIAN_POINT('Ctrl Pts',(3.00121933088198,-0.998125914862946,2.91133013131787));
#5686=CARTESIAN_POINT('Ctrl Pts',(3.00121933088198,-0.996867817321921,2.88623116420271));
#5687=CARTESIAN_POINT('Ctrl Pts',(3.00372567261398,-0.996197082307396,2.87284298569268));
#5688=CARTESIAN_POINT('Ctrl Pts',(3.01392742672708,-0.995249987974195,2.84820498168538));
#5689=CARTESIAN_POINT('Ctrl Pts',(3.02162367169069,-0.99498743710662,2.836954972072));
#5690=CARTESIAN_POINT('Ctrl Pts',(3.03939363383595,-0.99498743710662,2.81918500992674));
#5691=CARTESIAN_POINT('Ctrl Pts',(3.05064364344933,-0.995249987974195,2.81148876496312));
#5692=CARTESIAN_POINT('Ctrl Pts',(3.07528164745663,-0.996197082307396,2.80128701085003));
#5693=CARTESIAN_POINT('Ctrl Pts',(3.08866982596666,-0.996867817321921,2.79878066911803));
#5694=CARTESIAN_POINT('Ctrl Pts',(3.11376879308182,-0.998125914862946,2.79878066911803));
#5695=CARTESIAN_POINT('Ctrl Pts',(3.1271569976213,-0.99879518361721,2.80128700354859));
#5696=CARTESIAN_POINT('Ctrl Pts',(3.15179504543287,-0.999738921136592,2.81148877658419));
#5697=CARTESIAN_POINT('Ctrl Pts',(3.16304505817032,-1.,2.81918504016906));
#5698=CARTESIAN_POINT('Ctrl Pts',(3.17193000900063,-1.,2.82806999099937));
#5699=CARTESIAN_POINT('Ctrl Pts',(3.17193000900063,-1.,2.82806999099937));
#5700=CARTESIAN_POINT('Ctrl Pts',(3.18081495983094,-1.,2.83695494182968));
#5701=CARTESIAN_POINT('Ctrl Pts',(3.18851122341581,-0.999738921136592,2.84820495456713));
#5702=CARTESIAN_POINT('Ctrl Pts',(3.19871299645141,-0.99879518361721,2.8728430023787));
#5703=CARTESIAN_POINT('Ctrl Pts',(3.20121933088198,-0.998125914862946,2.88623120691819));
#5704=CARTESIAN_POINT('Ctrl Pts',(3.20121933088198,-0.996867817321921,2.91133017403334));
#5705=CARTESIAN_POINT('Ctrl Pts',(3.19871298914998,-0.996197082307396,2.92471835254337));
#5706=CARTESIAN_POINT('Ctrl Pts',(3.18851123503688,-0.995249987974195,2.94935635655067));
#5707=CARTESIAN_POINT('Ctrl Pts',(3.18081499007326,-0.99498743710662,2.96060636616405));
#5708=CARTESIAN_POINT('Ctrl Pts',(3.17193000900063,-0.99498743710662,2.96949134723668));
#5709=CARTESIAN_POINT('Origin',(3.10121933088198,-1.2,2.89878066911802));
#5710=CARTESIAN_POINT('',(3.17193000900063,0.99498743710662,2.96949134723668));
#5711=CARTESIAN_POINT('',(3.17193000900063,1.,2.82806999099937));
#5712=CARTESIAN_POINT('Ctrl Pts',(3.17193000900063,0.99498743710662,2.96949134723668));
#5713=CARTESIAN_POINT('Ctrl Pts',(3.18081499007326,0.99498743710662,2.96060636616405));
#5714=CARTESIAN_POINT('Ctrl Pts',(3.18851123503688,0.995249987974195,2.94935635655067));
#5715=CARTESIAN_POINT('Ctrl Pts',(3.19871298914998,0.996197082307397,2.92471835254337));
#5716=CARTESIAN_POINT('Ctrl Pts',(3.20121933088198,0.996867817321921,2.91133017403334));
#5717=CARTESIAN_POINT('Ctrl Pts',(3.20121933088198,0.998125914862946,2.88623120691818));
#5718=CARTESIAN_POINT('Ctrl Pts',(3.19871299645141,0.99879518361721,2.8728430023787));
#5719=CARTESIAN_POINT('Ctrl Pts',(3.18851122341581,0.999738921136592,2.84820495456713));
#5720=CARTESIAN_POINT('Ctrl Pts',(3.18081495983094,1.,2.83695494182968));
#5721=CARTESIAN_POINT('Ctrl Pts',(3.17193000900063,1.,2.82806999099937));
#5722=CARTESIAN_POINT('Ctrl Pts',(3.17193000900063,1.,2.82806999099937));
#5723=CARTESIAN_POINT('Ctrl Pts',(3.16304505817032,1.,2.81918504016906));
#5724=CARTESIAN_POINT('Ctrl Pts',(3.15179504543287,0.999738921136592,2.81148877658419));
#5725=CARTESIAN_POINT('Ctrl Pts',(3.1271569976213,0.99879518361721,2.80128700354859));
#5726=CARTESIAN_POINT('Ctrl Pts',(3.11376879308182,0.998125914862946,2.79878066911802));
#5727=CARTESIAN_POINT('Ctrl Pts',(3.08866982596666,0.996867817321921,2.79878066911803));
#5728=CARTESIAN_POINT('Ctrl Pts',(3.07528164745663,0.996197082307397,2.80128701085003));
#5729=CARTESIAN_POINT('Ctrl Pts',(3.05064364344933,0.995249987974195,2.81148876496312));
#5730=CARTESIAN_POINT('Ctrl Pts',(3.03939363383595,0.99498743710662,2.81918500992674));
#5731=CARTESIAN_POINT('Ctrl Pts',(3.02162367169069,0.99498743710662,2.836954972072));
#5732=CARTESIAN_POINT('Ctrl Pts',(3.01392742672708,0.995249987974195,2.84820498168538));
#5733=CARTESIAN_POINT('Ctrl Pts',(3.00372567261398,0.996197082307397,2.87284298569268));
#5734=CARTESIAN_POINT('Ctrl Pts',(3.00121933088198,0.996867817321921,2.88623116420271));
#5735=CARTESIAN_POINT('Ctrl Pts',(3.00121933088198,0.998125914862946,2.91133013131786));
#5736=CARTESIAN_POINT('Ctrl Pts',(3.00372566531254,0.99879518361721,2.92471833585735));
#5737=CARTESIAN_POINT('Ctrl Pts',(3.01392743834814,0.999738921136592,2.94935638366892));
#5738=CARTESIAN_POINT('Ctrl Pts',(3.02162370193301,1.,2.96060639640637));
#5739=CARTESIAN_POINT('Ctrl Pts',(3.03939360359363,1.,2.97837629806699));
#5740=CARTESIAN_POINT('Ctrl Pts',(3.05064361633108,0.999738921136592,2.98607256165186));
#5741=CARTESIAN_POINT('Ctrl Pts',(3.07528166414265,0.99879518361721,2.99627433468746));
#5742=CARTESIAN_POINT('Ctrl Pts',(3.08866986868214,0.998125914862946,2.99878066911802));
#5743=CARTESIAN_POINT('Ctrl Pts',(3.11376883579729,0.996867817321921,2.99878066911802));
#5744=CARTESIAN_POINT('Ctrl Pts',(3.12715701430732,0.996197082307397,2.99627432738602));
#5745=CARTESIAN_POINT('Ctrl Pts',(3.15179501831462,0.995249987974195,2.98607257327293));
#5746=CARTESIAN_POINT('Ctrl Pts',(3.163045027928,0.99498743710662,2.97837632830931));
#5747=CARTESIAN_POINT('Ctrl Pts',(3.17193000900063,0.99498743710662,2.96949134723668));
#5748=CARTESIAN_POINT('',(3.17193000900063,1.1,2.82806999099937));
#5749=CARTESIAN_POINT('',(3.17193000900063,-1.2,2.82806999099937));
#5750=CARTESIAN_POINT('',(3.17193000900063,1.09544511501033,2.96949134723668));
#5751=CARTESIAN_POINT('Ctrl Pts',(3.17193000900063,1.09544511501033,2.96949134723668));
#5752=CARTESIAN_POINT('Ctrl Pts',(3.16304614362663,1.09544511501033,2.97837521261068));
#5753=CARTESIAN_POINT('Ctrl Pts',(3.15179704377884,1.09568352051035,2.98607141763874));
#5754=CARTESIAN_POINT('Ctrl Pts',(3.12715904782386,1.09654384276605,2.99627380228311));
#5755=CARTESIAN_POINT('Ctrl Pts',(3.11377000115847,1.09715325263881,2.99878066911802));
#5756=CARTESIAN_POINT('Ctrl Pts',(3.08866868973591,1.09829658604435,2.99878066911802));
#5757=CARTESIAN_POINT('Ctrl Pts',(3.07527962532624,1.09890489533505,2.99627380720727));
#5758=CARTESIAN_POINT('Ctrl Pts',(3.05064159945906,1.09976269863984,2.986071409758));
#5759=CARTESIAN_POINT('Ctrl Pts',(3.03939249751764,1.1,2.978375191991));
#5760=CARTESIAN_POINT('Ctrl Pts',(3.021624808009,1.1,2.96060750248236));
#5761=CARTESIAN_POINT('Ctrl Pts',(3.013928590242,1.09976269863984,2.94935840054095));
#5762=CARTESIAN_POINT('Ctrl Pts',(3.00372619279273,1.09890489533505,2.92472037467376));
#5763=CARTESIAN_POINT('Ctrl Pts',(3.00121933088198,1.09829658604435,2.91133131026409));
#5764=CARTESIAN_POINT('Ctrl Pts',(3.00121933088198,1.09715325263881,2.88622999884153));
#5765=CARTESIAN_POINT('Ctrl Pts',(3.00372619771689,1.09654384276605,2.87284095217614));
#5766=CARTESIAN_POINT('Ctrl Pts',(3.01392858236127,1.09568352051035,2.84820295622116));
#5767=CARTESIAN_POINT('Ctrl Pts',(3.02162478738932,1.09544511501033,2.83695385637338));
#5768=CARTESIAN_POINT('Ctrl Pts',(3.03939251813733,1.09544511501033,2.81918612562536));
#5769=CARTESIAN_POINT('Ctrl Pts',(3.05064161798511,1.09568352051035,2.81148992059731));
#5770=CARTESIAN_POINT('Ctrl Pts',(3.07527961394009,1.09654384276605,2.80128753595294));
#5771=CARTESIAN_POINT('Ctrl Pts',(3.08866866060548,1.09715325263881,2.79878066911802));
#5772=CARTESIAN_POINT('Ctrl Pts',(3.11376997202804,1.09829658604435,2.79878066911802));
#5773=CARTESIAN_POINT('Ctrl Pts',(3.12715903643771,1.09890489533505,2.80128753102878));
#5774=CARTESIAN_POINT('Ctrl Pts',(3.1517970623049,1.09976269863984,2.81148992847805));
#5775=CARTESIAN_POINT('Ctrl Pts',(3.16304616424631,1.1,2.81918614624505));
#5776=CARTESIAN_POINT('Ctrl Pts',(3.17193000900063,1.1,2.82806999099937));
#5777=CARTESIAN_POINT('Ctrl Pts',(3.17193000900063,1.1,2.82806999099937));
#5778=CARTESIAN_POINT('Ctrl Pts',(3.18081385375495,1.1,2.83695383575369));
#5779=CARTESIAN_POINT('Ctrl Pts',(3.18851007152196,1.09976269863984,2.8482029376951));
#5780=CARTESIAN_POINT('Ctrl Pts',(3.19871246897122,1.09890489533505,2.87284096356229));
#5781=CARTESIAN_POINT('Ctrl Pts',(3.20121933088198,1.09829658604435,2.88623002797196));
#5782=CARTESIAN_POINT('Ctrl Pts',(3.20121933088198,1.09715325263881,2.91133133939452));
#5783=CARTESIAN_POINT('Ctrl Pts',(3.19871246404707,1.09654384276605,2.92472038605991));
#5784=CARTESIAN_POINT('Ctrl Pts',(3.18851007940269,1.09568352051035,2.94935838201489));
#5785=CARTESIAN_POINT('Ctrl Pts',(3.18081387437464,1.09544511501033,2.96060748186267));
#5786=CARTESIAN_POINT('Ctrl Pts',(3.17193000900063,1.09544511501033,2.96949134723668));
#5787=CARTESIAN_POINT('Origin',(1.9698484809835,-1.2,4.0301515190165));
#5788=CARTESIAN_POINT('',(2.04055915910216,-1.09544511501033,4.10086219713515));
#5789=CARTESIAN_POINT('',(2.04055915910216,-1.1,3.95944084089785));
#5790=CARTESIAN_POINT('Ctrl Pts',(2.04055915910216,-1.09544511501033,4.10086219713516));
#5791=CARTESIAN_POINT('Ctrl Pts',(2.04944302447616,-1.09544511501033,4.09197833176115));
#5792=CARTESIAN_POINT('Ctrl Pts',(2.05713922950421,-1.09568352051035,4.08072923191337));
#5793=CARTESIAN_POINT('Ctrl Pts',(2.06734161414859,-1.09654384276605,4.05609123595839));
#5794=CARTESIAN_POINT('Ctrl Pts',(2.0698484809835,-1.09715325263881,4.042702189293));
#5795=CARTESIAN_POINT('Ctrl Pts',(2.0698484809835,-1.09829658604435,4.01760087787044));
#5796=CARTESIAN_POINT('Ctrl Pts',(2.06734161907274,-1.09890489533505,4.00421181346076));
#5797=CARTESIAN_POINT('Ctrl Pts',(2.05713922162348,-1.09976269863984,3.97957378759358));
#5798=CARTESIAN_POINT('Ctrl Pts',(2.04944300385648,-1.1,3.96832468565217));
#5799=CARTESIAN_POINT('Ctrl Pts',(2.04055915910216,-1.1,3.95944084089785));
#5800=CARTESIAN_POINT('Ctrl Pts',(2.04055915910216,-1.1,3.95944084089785));
#5801=CARTESIAN_POINT('Ctrl Pts',(2.03167531434783,-1.1,3.95055699614353));
#5802=CARTESIAN_POINT('Ctrl Pts',(2.02042621240642,-1.09976269863984,3.94286077837652));
#5803=CARTESIAN_POINT('Ctrl Pts',(1.99578818653924,-1.09890489533505,3.93265838092726));
#5804=CARTESIAN_POINT('Ctrl Pts',(1.98239912212956,-1.09829658604435,3.9301515190165));
#5805=CARTESIAN_POINT('Ctrl Pts',(1.957297810707,-1.09715325263881,3.9301515190165));
#5806=CARTESIAN_POINT('Ctrl Pts',(1.94390876404161,-1.09654384276605,3.93265838585141));
#5807=CARTESIAN_POINT('Ctrl Pts',(1.91927076808664,-1.09568352051035,3.94286077049579));
#5808=CARTESIAN_POINT('Ctrl Pts',(1.90802166823885,-1.09544511501033,3.95055697552384));
#5809=CARTESIAN_POINT('Ctrl Pts',(1.89025393749084,-1.09544511501033,3.96832470627185));
#5810=CARTESIAN_POINT('Ctrl Pts',(1.88255773246279,-1.09568352051035,3.97957380611964));
#5811=CARTESIAN_POINT('Ctrl Pts',(1.87235534781841,-1.09654384276605,4.00421180207461));
#5812=CARTESIAN_POINT('Ctrl Pts',(1.8698484809835,-1.09715325263881,4.01760084874));
#5813=CARTESIAN_POINT('Ctrl Pts',(1.8698484809835,-1.09829658604435,4.04270216016256));
#5814=CARTESIAN_POINT('Ctrl Pts',(1.87235534289426,-1.09890489533505,4.05609122457224));
#5815=CARTESIAN_POINT('Ctrl Pts',(1.88255774034352,-1.09976269863984,4.08072925043942));
#5816=CARTESIAN_POINT('Ctrl Pts',(1.89025395811053,-1.1,4.09197835238083));
#5817=CARTESIAN_POINT('Ctrl Pts',(1.90802164761917,-1.1,4.10974604188948));
#5818=CARTESIAN_POINT('Ctrl Pts',(1.91927074956058,-1.09976269863984,4.11744225965648));
#5819=CARTESIAN_POINT('Ctrl Pts',(1.94390877542776,-1.09890489533505,4.12764465710574));
#5820=CARTESIAN_POINT('Ctrl Pts',(1.95729783983744,-1.09829658604435,4.1301515190165));
#5821=CARTESIAN_POINT('Ctrl Pts',(1.98239915126,-1.09715325263881,4.1301515190165));
#5822=CARTESIAN_POINT('Ctrl Pts',(1.99578819792539,-1.09654384276605,4.12764465218159));
#5823=CARTESIAN_POINT('Ctrl Pts',(2.02042619388036,-1.09568352051035,4.11744226753721));
#5824=CARTESIAN_POINT('Ctrl Pts',(2.03167529372815,-1.09544511501033,4.10974606250916));
#5825=CARTESIAN_POINT('Ctrl Pts',(2.04055915910215,-1.09544511501033,4.10086219713516));
#5826=CARTESIAN_POINT('',(2.04055915910215,-1.,3.95944084089785));
#5827=CARTESIAN_POINT('',(2.04055915910216,-1.2,3.95944084089785));
#5828=CARTESIAN_POINT('',(2.04055915910216,-0.99498743710662,4.10086219713516));
#5829=CARTESIAN_POINT('Ctrl Pts',(2.04055915910216,-0.99498743710662,4.10086219713516));
#5830=CARTESIAN_POINT('Ctrl Pts',(2.03167417802952,-0.99498743710662,4.10974717820779));
#5831=CARTESIAN_POINT('Ctrl Pts',(2.02042416841615,-0.995249987974195,4.1174434231714));
#5832=CARTESIAN_POINT('Ctrl Pts',(1.99578616440885,-0.996197082307396,4.1276451772845));
#5833=CARTESIAN_POINT('Ctrl Pts',(1.98239798589881,-0.996867817321921,4.1301515190165));
#5834=CARTESIAN_POINT('Ctrl Pts',(1.95729901878366,-0.998125914862946,4.1301515190165));
#5835=CARTESIAN_POINT('Ctrl Pts',(1.94391081424417,-0.99879518361721,4.12764518458593));
#5836=CARTESIAN_POINT('Ctrl Pts',(1.9192727664326,-0.999738921136592,4.11744341155034));
#5837=CARTESIAN_POINT('Ctrl Pts',(1.90802275369516,-1.,4.10974714796546));
#5838=CARTESIAN_POINT('Ctrl Pts',(1.89025285203454,-1.,4.09197724630485));
#5839=CARTESIAN_POINT('Ctrl Pts',(1.88255658844966,-0.999738921136592,4.0807272335674));
#5840=CARTESIAN_POINT('Ctrl Pts',(1.87235481541407,-0.99879518361721,4.05608918575583));
#5841=CARTESIAN_POINT('Ctrl Pts',(1.8698484809835,-0.998125914862946,4.04270098121634));
#5842=CARTESIAN_POINT('Ctrl Pts',(1.8698484809835,-0.996867817321921,4.01760201410119));
#5843=CARTESIAN_POINT('Ctrl Pts',(1.8723548227155,-0.996197082307396,4.00421383559115));
#5844=CARTESIAN_POINT('Ctrl Pts',(1.8825565768286,-0.995249987974195,3.97957583158386));
#5845=CARTESIAN_POINT('Ctrl Pts',(1.89025282179221,-0.99498743710662,3.96832582197048));
#5846=CARTESIAN_POINT('Ctrl Pts',(1.90802278393748,-0.99498743710662,3.95055585982521));
#5847=CARTESIAN_POINT('Ctrl Pts',(1.91927279355086,-0.995249987974195,3.9428596148616));
#5848=CARTESIAN_POINT('Ctrl Pts',(1.94391079755815,-0.996197082307396,3.9326578607485));
#5849=CARTESIAN_POINT('Ctrl Pts',(1.95729897606819,-0.996867817321921,3.9301515190165));
#5850=CARTESIAN_POINT('Ctrl Pts',(1.98239794318334,-0.998125914862946,3.9301515190165));
#5851=CARTESIAN_POINT('Ctrl Pts',(1.99578614772283,-0.99879518361721,3.93265785344707));
#5852=CARTESIAN_POINT('Ctrl Pts',(2.0204241955344,-0.999738921136592,3.94285962648266));
#5853=CARTESIAN_POINT('Ctrl Pts',(2.03167420827185,-1.,3.95055589006754));
#5854=CARTESIAN_POINT('Ctrl Pts',(2.04055915910216,-1.,3.95944084089785));
#5855=CARTESIAN_POINT('Ctrl Pts',(2.04055915910216,-1.,3.95944084089785));
#5856=CARTESIAN_POINT('Ctrl Pts',(2.04944410993246,-1.,3.96832579172816));
#5857=CARTESIAN_POINT('Ctrl Pts',(2.05714037351734,-0.999738921136592,3.9795758044656));
#5858=CARTESIAN_POINT('Ctrl Pts',(2.06734214655293,-0.99879518361721,4.00421385227717));
#5859=CARTESIAN_POINT('Ctrl Pts',(2.0698484809835,-0.998125914862946,4.01760205681666));
#5860=CARTESIAN_POINT('Ctrl Pts',(2.0698484809835,-0.996867817321921,4.04270102393181));
#5861=CARTESIAN_POINT('Ctrl Pts',(2.0673421392515,-0.996197082307396,4.05608920244185));
#5862=CARTESIAN_POINT('Ctrl Pts',(2.0571403851384,-0.995249987974195,4.08072720644915));
#5863=CARTESIAN_POINT('Ctrl Pts',(2.04944414017479,-0.99498743710662,4.09197721606252));
#5864=CARTESIAN_POINT('Ctrl Pts',(2.04055915910215,-0.99498743710662,4.10086219713516));
#5865=CARTESIAN_POINT('Origin',(1.9698484809835,-1.2,4.0301515190165));
#5866=CARTESIAN_POINT('',(2.04055915910216,0.99498743710662,4.10086219713516));
#5867=CARTESIAN_POINT('',(2.04055915910215,1.,3.95944084089785));
#5868=CARTESIAN_POINT('Ctrl Pts',(2.04055915910216,0.99498743710662,4.10086219713515));
#5869=CARTESIAN_POINT('Ctrl Pts',(2.04944414017479,0.99498743710662,4.09197721606252));
#5870=CARTESIAN_POINT('Ctrl Pts',(2.0571403851384,0.995249987974195,4.08072720644915));
#5871=CARTESIAN_POINT('Ctrl Pts',(2.0673421392515,0.996197082307397,4.05608920244185));
#5872=CARTESIAN_POINT('Ctrl Pts',(2.0698484809835,0.996867817321921,4.04270102393181));
#5873=CARTESIAN_POINT('Ctrl Pts',(2.0698484809835,0.998125914862946,4.01760205681666));
#5874=CARTESIAN_POINT('Ctrl Pts',(2.06734214655293,0.99879518361721,4.00421385227717));
#5875=CARTESIAN_POINT('Ctrl Pts',(2.05714037351734,0.999738921136592,3.9795758044656));
#5876=CARTESIAN_POINT('Ctrl Pts',(2.04944410993246,1.,3.96832579172816));
#5877=CARTESIAN_POINT('Ctrl Pts',(2.04055915910215,1.,3.95944084089785));
#5878=CARTESIAN_POINT('Ctrl Pts',(2.04055915910215,1.,3.95944084089785));
#5879=CARTESIAN_POINT('Ctrl Pts',(2.03167420827184,1.,3.95055589006754));
#5880=CARTESIAN_POINT('Ctrl Pts',(2.0204241955344,0.999738921136592,3.94285962648266));
#5881=CARTESIAN_POINT('Ctrl Pts',(1.99578614772283,0.99879518361721,3.93265785344707));
#5882=CARTESIAN_POINT('Ctrl Pts',(1.98239794318334,0.998125914862946,3.9301515190165));
#5883=CARTESIAN_POINT('Ctrl Pts',(1.95729897606819,0.996867817321921,3.9301515190165));
#5884=CARTESIAN_POINT('Ctrl Pts',(1.94391079755815,0.996197082307397,3.9326578607485));
#5885=CARTESIAN_POINT('Ctrl Pts',(1.91927279355086,0.995249987974195,3.9428596148616));
#5886=CARTESIAN_POINT('Ctrl Pts',(1.90802278393748,0.99498743710662,3.95055585982521));
#5887=CARTESIAN_POINT('Ctrl Pts',(1.89025282179221,0.99498743710662,3.96832582197048));
#5888=CARTESIAN_POINT('Ctrl Pts',(1.8825565768286,0.995249987974195,3.97957583158386));
#5889=CARTESIAN_POINT('Ctrl Pts',(1.8723548227155,0.996197082307397,4.00421383559115));
#5890=CARTESIAN_POINT('Ctrl Pts',(1.8698484809835,0.996867817321921,4.01760201410119));
#5891=CARTESIAN_POINT('Ctrl Pts',(1.8698484809835,0.998125914862946,4.04270098121634));
#5892=CARTESIAN_POINT('Ctrl Pts',(1.87235481541407,0.99879518361721,4.05608918575583));
#5893=CARTESIAN_POINT('Ctrl Pts',(1.88255658844966,0.999738921136592,4.0807272335674));
#5894=CARTESIAN_POINT('Ctrl Pts',(1.89025285203454,1.,4.09197724630484));
#5895=CARTESIAN_POINT('Ctrl Pts',(1.90802275369516,1.,4.10974714796546));
#5896=CARTESIAN_POINT('Ctrl Pts',(1.9192727664326,0.999738921136592,4.11744341155034));
#5897=CARTESIAN_POINT('Ctrl Pts',(1.94391081424417,0.99879518361721,4.12764518458593));
#5898=CARTESIAN_POINT('Ctrl Pts',(1.95729901878366,0.998125914862946,4.1301515190165));
#5899=CARTESIAN_POINT('Ctrl Pts',(1.98239798589881,0.996867817321921,4.1301515190165));
#5900=CARTESIAN_POINT('Ctrl Pts',(1.99578616440885,0.996197082307397,4.1276451772845));
#5901=CARTESIAN_POINT('Ctrl Pts',(2.02042416841614,0.995249987974195,4.1174434231714));
#5902=CARTESIAN_POINT('Ctrl Pts',(2.03167417802952,0.99498743710662,4.10974717820779));
#5903=CARTESIAN_POINT('Ctrl Pts',(2.04055915910215,0.99498743710662,4.10086219713516));
#5904=CARTESIAN_POINT('',(2.04055915910215,1.1,3.95944084089785));
#5905=CARTESIAN_POINT('',(2.04055915910216,-1.2,3.95944084089785));
#5906=CARTESIAN_POINT('',(2.04055915910215,1.09544511501033,4.10086219713516));
#5907=CARTESIAN_POINT('Ctrl Pts',(2.04055915910216,1.09544511501033,4.10086219713515));
#5908=CARTESIAN_POINT('Ctrl Pts',(2.03167529372815,1.09544511501033,4.10974606250916));
#5909=CARTESIAN_POINT('Ctrl Pts',(2.02042619388037,1.09568352051035,4.11744226753721));
#5910=CARTESIAN_POINT('Ctrl Pts',(1.99578819792539,1.09654384276605,4.12764465218159));
#5911=CARTESIAN_POINT('Ctrl Pts',(1.98239915126,1.09715325263881,4.1301515190165));
#5912=CARTESIAN_POINT('Ctrl Pts',(1.95729783983744,1.09829658604435,4.1301515190165));
#5913=CARTESIAN_POINT('Ctrl Pts',(1.94390877542776,1.09890489533505,4.12764465710574));
#5914=CARTESIAN_POINT('Ctrl Pts',(1.91927074956058,1.09976269863984,4.11744225965648));
#5915=CARTESIAN_POINT('Ctrl Pts',(1.90802164761917,1.1,4.10974604188948));
#5916=CARTESIAN_POINT('Ctrl Pts',(1.89025395811052,1.1,4.09197835238083));
#5917=CARTESIAN_POINT('Ctrl Pts',(1.88255774034352,1.09976269863984,4.08072925043942));
#5918=CARTESIAN_POINT('Ctrl Pts',(1.87235534289426,1.09890489533505,4.05609122457224));
#5919=CARTESIAN_POINT('Ctrl Pts',(1.8698484809835,1.09829658604435,4.04270216016256));
#5920=CARTESIAN_POINT('Ctrl Pts',(1.8698484809835,1.09715325263881,4.01760084874));
#5921=CARTESIAN_POINT('Ctrl Pts',(1.87235534781841,1.09654384276605,4.00421180207461));
#5922=CARTESIAN_POINT('Ctrl Pts',(1.88255773246279,1.09568352051035,3.97957380611964));
#5923=CARTESIAN_POINT('Ctrl Pts',(1.89025393749084,1.09544511501033,3.96832470627185));
#5924=CARTESIAN_POINT('Ctrl Pts',(1.90802166823885,1.09544511501033,3.95055697552384));
#5925=CARTESIAN_POINT('Ctrl Pts',(1.91927076808664,1.09568352051035,3.94286077049579));
#5926=CARTESIAN_POINT('Ctrl Pts',(1.94390876404161,1.09654384276605,3.93265838585141));
#5927=CARTESIAN_POINT('Ctrl Pts',(1.957297810707,1.09715325263881,3.9301515190165));
#5928=CARTESIAN_POINT('Ctrl Pts',(1.98239912212956,1.09829658604435,3.9301515190165));
#5929=CARTESIAN_POINT('Ctrl Pts',(1.99578818653924,1.09890489533505,3.93265838092726));
#5930=CARTESIAN_POINT('Ctrl Pts',(2.02042621240642,1.09976269863984,3.94286077837652));
#5931=CARTESIAN_POINT('Ctrl Pts',(2.03167531434783,1.1,3.95055699614353));
#5932=CARTESIAN_POINT('Ctrl Pts',(2.04055915910215,1.1,3.95944084089785));
#5933=CARTESIAN_POINT('Ctrl Pts',(2.04055915910215,1.1,3.95944084089785));
#5934=CARTESIAN_POINT('Ctrl Pts',(2.04944300385648,1.1,3.96832468565217));
#5935=CARTESIAN_POINT('Ctrl Pts',(2.05713922162348,1.09976269863984,3.97957378759358));
#5936=CARTESIAN_POINT('Ctrl Pts',(2.06734161907274,1.09890489533505,4.00421181346076));
#5937=CARTESIAN_POINT('Ctrl Pts',(2.0698484809835,1.09829658604435,4.01760087787044));
#5938=CARTESIAN_POINT('Ctrl Pts',(2.0698484809835,1.09715325263881,4.042702189293));
#5939=CARTESIAN_POINT('Ctrl Pts',(2.06734161414859,1.09654384276605,4.05609123595839));
#5940=CARTESIAN_POINT('Ctrl Pts',(2.05713922950421,1.09568352051035,4.08072923191336));
#5941=CARTESIAN_POINT('Ctrl Pts',(2.04944302447616,1.09544511501033,4.09197833176115));
#5942=CARTESIAN_POINT('Ctrl Pts',(2.04055915910215,1.09544511501033,4.10086219713516));
#5943=CARTESIAN_POINT('Origin',(1.40416305603426,-1.2,4.59583694396574));
#5944=CARTESIAN_POINT('',(1.47487373415292,-1.09544511501033,4.66654762208439));
#5945=CARTESIAN_POINT('',(1.47487373415292,-1.1,4.52512626584708));
#5946=CARTESIAN_POINT('Ctrl Pts',(1.47487373415292,-1.09544511501033,4.66654762208439));
#5947=CARTESIAN_POINT('Ctrl Pts',(1.48375759952692,-1.09544511501033,4.65766375671039));
#5948=CARTESIAN_POINT('Ctrl Pts',(1.49145380455497,-1.09568352051035,4.64641465686261));
#5949=CARTESIAN_POINT('Ctrl Pts',(1.50165618919935,-1.09654384276605,4.62177666090763));
#5950=CARTESIAN_POINT('Ctrl Pts',(1.50416305603426,-1.09715325263881,4.60838761424224));
#5951=CARTESIAN_POINT('Ctrl Pts',(1.50416305603426,-1.09829658604435,4.58328630281968));
#5952=CARTESIAN_POINT('Ctrl Pts',(1.50165619412351,-1.09890489533505,4.56989723841));
#5953=CARTESIAN_POINT('Ctrl Pts',(1.49145379667424,-1.09976269863984,4.54525921254282));
#5954=CARTESIAN_POINT('Ctrl Pts',(1.48375757890724,-1.1,4.5340101106014));
#5955=CARTESIAN_POINT('Ctrl Pts',(1.47487373415292,-1.1,4.52512626584708));
#5956=CARTESIAN_POINT('Ctrl Pts',(1.47487373415292,-1.1,4.52512626584708));
#5957=CARTESIAN_POINT('Ctrl Pts',(1.4659898893986,-1.1,4.51624242109276));
#5958=CARTESIAN_POINT('Ctrl Pts',(1.45474078745718,-1.09976269863984,4.50854620332576));
#5959=CARTESIAN_POINT('Ctrl Pts',(1.43010276159,-1.09890489533505,4.49834380587649));
#5960=CARTESIAN_POINT('Ctrl Pts',(1.41671369718032,-1.09829658604435,4.49583694396574));
#5961=CARTESIAN_POINT('Ctrl Pts',(1.39161238575777,-1.09715325263881,4.49583694396574));
#5962=CARTESIAN_POINT('Ctrl Pts',(1.37822333909238,-1.09654384276605,4.49834381080065));
#5963=CARTESIAN_POINT('Ctrl Pts',(1.3535853431374,-1.09568352051035,4.50854619544503));
#5964=CARTESIAN_POINT('Ctrl Pts',(1.34233624328961,-1.09544511501033,4.51624240047308));
#5965=CARTESIAN_POINT('Ctrl Pts',(1.3245685125416,-1.09544511501033,4.53401013122109));
#5966=CARTESIAN_POINT('Ctrl Pts',(1.31687230751355,-1.09568352051035,4.54525923106887));
#5967=CARTESIAN_POINT('Ctrl Pts',(1.30666992286917,-1.09654384276605,4.56989722702385));
#5968=CARTESIAN_POINT('Ctrl Pts',(1.30416305603426,-1.09715325263881,4.58328627368924));
#5969=CARTESIAN_POINT('Ctrl Pts',(1.30416305603426,-1.09829658604435,4.6083875851118));
#5970=CARTESIAN_POINT('Ctrl Pts',(1.30666991794502,-1.09890489533505,4.62177664952148));
#5971=CARTESIAN_POINT('Ctrl Pts',(1.31687231539428,-1.09976269863984,4.64641467538866));
#5972=CARTESIAN_POINT('Ctrl Pts',(1.32456853316129,-1.1,4.65766377733007));
#5973=CARTESIAN_POINT('Ctrl Pts',(1.34233622266993,-1.1,4.67543146683871));
#5974=CARTESIAN_POINT('Ctrl Pts',(1.35358532461134,-1.09976269863984,4.68312768460572));
#5975=CARTESIAN_POINT('Ctrl Pts',(1.37822335047852,-1.09890489533505,4.69333008205498));
#5976=CARTESIAN_POINT('Ctrl Pts',(1.3916124148882,-1.09829658604435,4.69583694396574));
#5977=CARTESIAN_POINT('Ctrl Pts',(1.41671372631076,-1.09715325263881,4.69583694396574));
#5978=CARTESIAN_POINT('Ctrl Pts',(1.43010277297615,-1.09654384276605,4.69333007713083));
#5979=CARTESIAN_POINT('Ctrl Pts',(1.45474076893113,-1.09568352051035,4.68312769248645));
#5980=CARTESIAN_POINT('Ctrl Pts',(1.46598986877891,-1.09544511501033,4.6754314874584));
#5981=CARTESIAN_POINT('Ctrl Pts',(1.47487373415292,-1.09544511501033,4.66654762208439));
#5982=CARTESIAN_POINT('',(1.47487373415292,-1.,4.52512626584708));
#5983=CARTESIAN_POINT('',(1.47487373415292,-1.2,4.52512626584708));
#5984=CARTESIAN_POINT('',(1.47487373415292,-0.99498743710662,4.66654762208439));
#5985=CARTESIAN_POINT('Ctrl Pts',(1.47487373415292,-0.99498743710662,4.66654762208439));
#5986=CARTESIAN_POINT('Ctrl Pts',(1.46598875308029,-0.99498743710662,4.67543260315702));
#5987=CARTESIAN_POINT('Ctrl Pts',(1.45473874346691,-0.995249987974195,4.68312884812064));
#5988=CARTESIAN_POINT('Ctrl Pts',(1.43010073945961,-0.996197082307396,4.69333060223374));
#5989=CARTESIAN_POINT('Ctrl Pts',(1.41671256094958,-0.996867817321921,4.69583694396574));
#5990=CARTESIAN_POINT('Ctrl Pts',(1.39161359383442,-0.998125914862946,4.69583694396574));
#5991=CARTESIAN_POINT('Ctrl Pts',(1.37822538929493,-0.99879518361721,4.69333060953517));
#5992=CARTESIAN_POINT('Ctrl Pts',(1.35358734148336,-0.999738921136592,4.68312883649958));
#5993=CARTESIAN_POINT('Ctrl Pts',(1.34233732874592,-1.,4.6754325729147));
#5994=CARTESIAN_POINT('Ctrl Pts',(1.3245674270853,-1.,4.65766267125408));
#5995=CARTESIAN_POINT('Ctrl Pts',(1.31687116350042,-0.999738921136592,4.64641265851664));
#5996=CARTESIAN_POINT('Ctrl Pts',(1.30666939046483,-0.99879518361721,4.62177461070507));
#5997=CARTESIAN_POINT('Ctrl Pts',(1.30416305603426,-0.998125914862946,4.60838640616558));
#5998=CARTESIAN_POINT('Ctrl Pts',(1.30416305603426,-0.996867817321921,4.58328743905042));
#5999=CARTESIAN_POINT('Ctrl Pts',(1.30666939776626,-0.996197082307396,4.56989926054039));
#6000=CARTESIAN_POINT('Ctrl Pts',(1.31687115187936,-0.995249987974195,4.54526125653309));
#6001=CARTESIAN_POINT('Ctrl Pts',(1.32456739684298,-0.99498743710662,4.53401124691971));
#6002=CARTESIAN_POINT('Ctrl Pts',(1.34233735898824,-0.99498743710662,4.51624128477445));
#6003=CARTESIAN_POINT('Ctrl Pts',(1.35358736860162,-0.995249987974195,4.50854503981084));
#6004=CARTESIAN_POINT('Ctrl Pts',(1.37822537260892,-0.996197082307397,4.49834328569774));
#6005=CARTESIAN_POINT('Ctrl Pts',(1.39161355111895,-0.996867817321921,4.49583694396574));
#6006=CARTESIAN_POINT('Ctrl Pts',(1.4167125182341,-0.998125914862946,4.49583694396574));
#6007=CARTESIAN_POINT('Ctrl Pts',(1.43010072277359,-0.99879518361721,4.49834327839631));
#6008=CARTESIAN_POINT('Ctrl Pts',(1.45473877058516,-0.999738921136592,4.5085450514319));
#6009=CARTESIAN_POINT('Ctrl Pts',(1.46598878332261,-1.,4.51624131501677));
#6010=CARTESIAN_POINT('Ctrl Pts',(1.47487373415292,-1.,4.52512626584708));
#6011=CARTESIAN_POINT('Ctrl Pts',(1.47487373415292,-1.,4.52512626584708));
#6012=CARTESIAN_POINT('Ctrl Pts',(1.48375868498323,-1.,4.53401121667739));
#6013=CARTESIAN_POINT('Ctrl Pts',(1.4914549485681,-0.999738921136592,4.54526122941484));
#6014=CARTESIAN_POINT('Ctrl Pts',(1.50165672160369,-0.99879518361721,4.56989927722641));
#6015=CARTESIAN_POINT('Ctrl Pts',(1.50416305603426,-0.998125914862946,4.5832874817659));
#6016=CARTESIAN_POINT('Ctrl Pts',(1.50416305603426,-0.996867817321921,4.60838644888105));
#6017=CARTESIAN_POINT('Ctrl Pts',(1.50165671430226,-0.996197082307396,4.62177462739109));
#6018=CARTESIAN_POINT('Ctrl Pts',(1.49145496018916,-0.995249987974195,4.64641263139838));
#6019=CARTESIAN_POINT('Ctrl Pts',(1.48375871522555,-0.99498743710662,4.65766264101176));
#6020=CARTESIAN_POINT('Ctrl Pts',(1.47487373415292,-0.99498743710662,4.66654762208439));
#6021=CARTESIAN_POINT('Origin',(1.40416305603426,-1.2,4.59583694396574));
#6022=CARTESIAN_POINT('',(1.47487373415292,0.99498743710662,4.66654762208439));
#6023=CARTESIAN_POINT('',(1.47487373415292,1.,4.52512626584708));
#6024=CARTESIAN_POINT('Ctrl Pts',(1.47487373415292,0.99498743710662,4.66654762208439));
#6025=CARTESIAN_POINT('Ctrl Pts',(1.48375871522555,0.99498743710662,4.65766264101176));
#6026=CARTESIAN_POINT('Ctrl Pts',(1.49145496018916,0.995249987974195,4.64641263139838));
#6027=CARTESIAN_POINT('Ctrl Pts',(1.50165671430226,0.996197082307397,4.62177462739108));
#6028=CARTESIAN_POINT('Ctrl Pts',(1.50416305603426,0.996867817321921,4.60838644888105));
#6029=CARTESIAN_POINT('Ctrl Pts',(1.50416305603426,0.998125914862946,4.5832874817659));
#6030=CARTESIAN_POINT('Ctrl Pts',(1.50165672160369,0.99879518361721,4.56989927722641));
#6031=CARTESIAN_POINT('Ctrl Pts',(1.4914549485681,0.999738921136592,4.54526122941484));
#6032=CARTESIAN_POINT('Ctrl Pts',(1.48375868498323,1.,4.53401121667739));
#6033=CARTESIAN_POINT('Ctrl Pts',(1.47487373415292,1.,4.52512626584708));
#6034=CARTESIAN_POINT('Ctrl Pts',(1.47487373415292,1.,4.52512626584708));
#6035=CARTESIAN_POINT('Ctrl Pts',(1.46598878332261,1.,4.51624131501678));
#6036=CARTESIAN_POINT('Ctrl Pts',(1.45473877058516,0.999738921136592,4.5085450514319));
#6037=CARTESIAN_POINT('Ctrl Pts',(1.43010072277359,0.99879518361721,4.49834327839631));
#6038=CARTESIAN_POINT('Ctrl Pts',(1.4167125182341,0.998125914862946,4.49583694396574));
#6039=CARTESIAN_POINT('Ctrl Pts',(1.39161355111895,0.996867817321921,4.49583694396574));
#6040=CARTESIAN_POINT('Ctrl Pts',(1.37822537260892,0.996197082307397,4.49834328569774));
#6041=CARTESIAN_POINT('Ctrl Pts',(1.35358736860162,0.995249987974195,4.50854503981084));
#6042=CARTESIAN_POINT('Ctrl Pts',(1.34233735898824,0.99498743710662,4.51624128477445));
#6043=CARTESIAN_POINT('Ctrl Pts',(1.32456739684298,0.99498743710662,4.53401124691971));
#6044=CARTESIAN_POINT('Ctrl Pts',(1.31687115187936,0.995249987974195,4.54526125653309));
#6045=CARTESIAN_POINT('Ctrl Pts',(1.30666939776626,0.996197082307397,4.56989926054039));
#6046=CARTESIAN_POINT('Ctrl Pts',(1.30416305603426,0.996867817321921,4.58328743905042));
#6047=CARTESIAN_POINT('Ctrl Pts',(1.30416305603426,0.998125914862946,4.60838640616558));
#6048=CARTESIAN_POINT('Ctrl Pts',(1.30666939046483,0.99879518361721,4.62177461070507));
#6049=CARTESIAN_POINT('Ctrl Pts',(1.31687116350042,0.999738921136592,4.64641265851664));
#6050=CARTESIAN_POINT('Ctrl Pts',(1.3245674270853,1.,4.65766267125408));
#6051=CARTESIAN_POINT('Ctrl Pts',(1.34233732874592,1.,4.6754325729147));
#6052=CARTESIAN_POINT('Ctrl Pts',(1.35358734148336,0.999738921136592,4.68312883649958));
#6053=CARTESIAN_POINT('Ctrl Pts',(1.37822538929493,0.99879518361721,4.69333060953517));
#6054=CARTESIAN_POINT('Ctrl Pts',(1.39161359383442,0.998125914862946,4.69583694396574));
#6055=CARTESIAN_POINT('Ctrl Pts',(1.41671256094958,0.996867817321921,4.69583694396574));
#6056=CARTESIAN_POINT('Ctrl Pts',(1.43010073945961,0.996197082307397,4.69333060223374));
#6057=CARTESIAN_POINT('Ctrl Pts',(1.45473874346691,0.995249987974195,4.68312884812064));
#6058=CARTESIAN_POINT('Ctrl Pts',(1.46598875308029,0.99498743710662,4.67543260315702));
#6059=CARTESIAN_POINT('Ctrl Pts',(1.47487373415292,0.99498743710662,4.66654762208439));
#6060=CARTESIAN_POINT('',(1.47487373415292,1.1,4.52512626584708));
#6061=CARTESIAN_POINT('',(1.47487373415292,-1.2,4.52512626584708));
#6062=CARTESIAN_POINT('',(1.47487373415292,1.09544511501033,4.66654762208439));
#6063=CARTESIAN_POINT('Ctrl Pts',(1.47487373415292,1.09544511501033,4.66654762208439));
#6064=CARTESIAN_POINT('Ctrl Pts',(1.46598986877891,1.09544511501033,4.6754314874584));
#6065=CARTESIAN_POINT('Ctrl Pts',(1.45474076893113,1.09568352051035,4.68312769248645));
#6066=CARTESIAN_POINT('Ctrl Pts',(1.43010277297615,1.09654384276605,4.69333007713083));
#6067=CARTESIAN_POINT('Ctrl Pts',(1.41671372631076,1.09715325263881,4.69583694396574));
#6068=CARTESIAN_POINT('Ctrl Pts',(1.3916124148882,1.09829658604435,4.69583694396574));
#6069=CARTESIAN_POINT('Ctrl Pts',(1.37822335047852,1.09890489533505,4.69333008205498));
#6070=CARTESIAN_POINT('Ctrl Pts',(1.35358532461134,1.09976269863984,4.68312768460572));
#6071=CARTESIAN_POINT('Ctrl Pts',(1.34233622266993,1.1,4.67543146683871));
#6072=CARTESIAN_POINT('Ctrl Pts',(1.32456853316129,1.1,4.65766377733007));
#6073=CARTESIAN_POINT('Ctrl Pts',(1.31687231539428,1.09976269863984,4.64641467538866));
#6074=CARTESIAN_POINT('Ctrl Pts',(1.30666991794502,1.09890489533505,4.62177664952148));
#6075=CARTESIAN_POINT('Ctrl Pts',(1.30416305603426,1.09829658604435,4.6083875851118));
#6076=CARTESIAN_POINT('Ctrl Pts',(1.30416305603426,1.09715325263881,4.58328627368924));
#6077=CARTESIAN_POINT('Ctrl Pts',(1.30666992286917,1.09654384276605,4.56989722702385));
#6078=CARTESIAN_POINT('Ctrl Pts',(1.31687230751355,1.09568352051035,4.54525923106887));
#6079=CARTESIAN_POINT('Ctrl Pts',(1.3245685125416,1.09544511501033,4.53401013122109));
#6080=CARTESIAN_POINT('Ctrl Pts',(1.34233624328961,1.09544511501033,4.51624240047308));
#6081=CARTESIAN_POINT('Ctrl Pts',(1.3535853431374,1.09568352051035,4.50854619544503));
#6082=CARTESIAN_POINT('Ctrl Pts',(1.37822333909238,1.09654384276605,4.49834381080065));
#6083=CARTESIAN_POINT('Ctrl Pts',(1.39161238575776,1.09715325263881,4.49583694396574));
#6084=CARTESIAN_POINT('Ctrl Pts',(1.41671369718032,1.09829658604435,4.49583694396574));
#6085=CARTESIAN_POINT('Ctrl Pts',(1.43010276159,1.09890489533505,4.49834380587649));
#6086=CARTESIAN_POINT('Ctrl Pts',(1.45474078745718,1.09976269863984,4.50854620332576));
#6087=CARTESIAN_POINT('Ctrl Pts',(1.4659898893986,1.1,4.51624242109276));
#6088=CARTESIAN_POINT('Ctrl Pts',(1.47487373415292,1.1,4.52512626584708));
#6089=CARTESIAN_POINT('Ctrl Pts',(1.47487373415292,1.1,4.52512626584708));
#6090=CARTESIAN_POINT('Ctrl Pts',(1.48375757890724,1.1,4.5340101106014));
#6091=CARTESIAN_POINT('Ctrl Pts',(1.49145379667424,1.09976269863984,4.54525921254282));
#6092=CARTESIAN_POINT('Ctrl Pts',(1.50165619412351,1.09890489533505,4.56989723841));
#6093=CARTESIAN_POINT('Ctrl Pts',(1.50416305603426,1.09829658604435,4.58328630281968));
#6094=CARTESIAN_POINT('Ctrl Pts',(1.50416305603426,1.09715325263881,4.60838761424224));
#6095=CARTESIAN_POINT('Ctrl Pts',(1.50165618919935,1.09654384276605,4.62177666090763));
#6096=CARTESIAN_POINT('Ctrl Pts',(1.49145380455497,1.09568352051035,4.64641465686261));
#6097=CARTESIAN_POINT('Ctrl Pts',(1.48375759952692,1.09544511501033,4.65766375671039));
#6098=CARTESIAN_POINT('Ctrl Pts',(1.47487373415292,1.09544511501033,4.66654762208439));
#6099=CARTESIAN_POINT('Origin',(0.838477631085024,-1.2,5.16152236891498));
#6100=CARTESIAN_POINT('',(0.909188309203679,-1.09544511501033,5.23223304703363));
#6101=CARTESIAN_POINT('',(0.909188309203679,-1.1,5.09081169079632));
#6102=CARTESIAN_POINT('Ctrl Pts',(0.909188309203679,-1.09544511501033,5.23223304703363));
#6103=CARTESIAN_POINT('Ctrl Pts',(0.918072174577685,-1.09544511501033,5.22334918165963));
#6104=CARTESIAN_POINT('Ctrl Pts',(0.925768379605735,-1.09568352051035,5.21210008181184));
#6105=CARTESIAN_POINT('Ctrl Pts',(0.935970764250114,-1.09654384276605,5.18746208585686));
#6106=CARTESIAN_POINT('Ctrl Pts',(0.938477631085024,-1.09715325263881,5.17407303919147));
#6107=CARTESIAN_POINT('Ctrl Pts',(0.938477631085024,-1.09829658604435,5.14897172776891));
#6108=CARTESIAN_POINT('Ctrl Pts',(0.93597076917427,-1.09890489533505,5.13558266335924));
#6109=CARTESIAN_POINT('Ctrl Pts',(0.925768371725004,-1.09976269863984,5.11094463749205));
#6110=CARTESIAN_POINT('Ctrl Pts',(0.918072153958,-1.1,5.09969553555064));
#6111=CARTESIAN_POINT('Ctrl Pts',(0.909188309203679,-1.1,5.09081169079632));
#6112=CARTESIAN_POINT('Ctrl Pts',(0.909188309203679,-1.1,5.09081169079632));
#6113=CARTESIAN_POINT('Ctrl Pts',(0.900304464449358,-1.1,5.081927846042));
#6114=CARTESIAN_POINT('Ctrl Pts',(0.889055362507946,-1.09976269863984,5.074231628275));
#6115=CARTESIAN_POINT('Ctrl Pts',(0.864417336640763,-1.09890489533505,5.06402923082573));
#6116=CARTESIAN_POINT('Ctrl Pts',(0.851028272231086,-1.09829658604435,5.06152236891498));
#6117=CARTESIAN_POINT('Ctrl Pts',(0.825926960808528,-1.09715325263881,5.06152236891498));
#6118=CARTESIAN_POINT('Ctrl Pts',(0.812537914143138,-1.09654384276605,5.06402923574989));
#6119=CARTESIAN_POINT('Ctrl Pts',(0.787899918188158,-1.09568352051035,5.07423162039427));
#6120=CARTESIAN_POINT('Ctrl Pts',(0.776650818340375,-1.09544511501033,5.08192782542232));
#6121=CARTESIAN_POINT('Ctrl Pts',(0.758883087592364,-1.09544511501033,5.09969555617033));
#6122=CARTESIAN_POINT('Ctrl Pts',(0.751186882564314,-1.09568352051035,5.11094465601811));
#6123=CARTESIAN_POINT('Ctrl Pts',(0.740984497919935,-1.09654384276605,5.13558265197309));
#6124=CARTESIAN_POINT('Ctrl Pts',(0.738477631085024,-1.09715325263881,5.14897169863848));
#6125=CARTESIAN_POINT('Ctrl Pts',(0.738477631085024,-1.09829658604435,5.17407301006104));
#6126=CARTESIAN_POINT('Ctrl Pts',(0.740984492995779,-1.09890489533505,5.18746207447071));
#6127=CARTESIAN_POINT('Ctrl Pts',(0.751186890445044,-1.09976269863984,5.2121001003379));
#6128=CARTESIAN_POINT('Ctrl Pts',(0.758883108212049,-1.1,5.22334920227931));
#6129=CARTESIAN_POINT('Ctrl Pts',(0.77665079772069,-1.1,5.24111689178795));
#6130=CARTESIAN_POINT('Ctrl Pts',(0.787899899662102,-1.09976269863984,5.24881310955496));
#6131=CARTESIAN_POINT('Ctrl Pts',(0.812537925529286,-1.09890489533505,5.25901550700422));
#6132=CARTESIAN_POINT('Ctrl Pts',(0.825926989938963,-1.09829658604435,5.26152236891498));
#6133=CARTESIAN_POINT('Ctrl Pts',(0.851028301361521,-1.09715325263881,5.26152236891498));
#6134=CARTESIAN_POINT('Ctrl Pts',(0.864417348026911,-1.09654384276605,5.25901550208007));
#6135=CARTESIAN_POINT('Ctrl Pts',(0.88905534398189,-1.09568352051035,5.24881311743569));
#6136=CARTESIAN_POINT('Ctrl Pts',(0.900304443829673,-1.09544511501033,5.24111691240764));
#6137=CARTESIAN_POINT('Ctrl Pts',(0.909188309203679,-1.09544511501033,5.23223304703363));
#6138=CARTESIAN_POINT('',(0.909188309203679,-1.,5.09081169079632));
#6139=CARTESIAN_POINT('',(0.909188309203679,-1.2,5.09081169079632));
#6140=CARTESIAN_POINT('',(0.909188309203679,-0.99498743710662,5.23223304703363));
#6141=CARTESIAN_POINT('Ctrl Pts',(0.909188309203679,-0.99498743710662,5.23223304703363));
#6142=CARTESIAN_POINT('Ctrl Pts',(0.900303328131047,-0.99498743710662,5.24111802810626));
#6143=CARTESIAN_POINT('Ctrl Pts',(0.889053318517669,-0.995249987974195,
5.24881427306988));
#6144=CARTESIAN_POINT('Ctrl Pts',(0.864415314510371,-0.996197082307396,
5.25901602718298));
#6145=CARTESIAN_POINT('Ctrl Pts',(0.851027136000337,-0.996867817321921,
5.26152236891498));
#6146=CARTESIAN_POINT('Ctrl Pts',(0.825928168885184,-0.998125914862946,
5.26152236891498));
#6147=CARTESIAN_POINT('Ctrl Pts',(0.812539964345697,-0.99879518361721,5.25901603448441));
#6148=CARTESIAN_POINT('Ctrl Pts',(0.787901916534127,-0.999738921136592,
5.24881426144881));
#6149=CARTESIAN_POINT('Ctrl Pts',(0.776651903796679,-1.,5.24111799786394));
#6150=CARTESIAN_POINT('Ctrl Pts',(0.75888200213606,-1.,5.22334809620332));
#6151=CARTESIAN_POINT('Ctrl Pts',(0.751185738551187,-0.999738921136592,
5.21209808346587));
#6152=CARTESIAN_POINT('Ctrl Pts',(0.740983965515592,-0.99879518361721,5.1874600356543));
#6153=CARTESIAN_POINT('Ctrl Pts',(0.738477631085025,-0.998125914862946,
5.17407183111482));
#6154=CARTESIAN_POINT('Ctrl Pts',(0.738477631085024,-0.996867817321921,
5.14897286399966));
#6155=CARTESIAN_POINT('Ctrl Pts',(0.740983972817025,-0.996197082307396,
5.13558468548963));
#6156=CARTESIAN_POINT('Ctrl Pts',(0.751185726930123,-0.995249987974195,
5.11094668148233));
#6157=CARTESIAN_POINT('Ctrl Pts',(0.758881971893738,-0.99498743710662,5.09969667186895));
#6158=CARTESIAN_POINT('Ctrl Pts',(0.776651934039001,-0.99498743710662,5.08192670972369));
#6159=CARTESIAN_POINT('Ctrl Pts',(0.78790194365238,-0.995249987974195,5.07423046476008));
#6160=CARTESIAN_POINT('Ctrl Pts',(0.812539947659678,-0.996197082307396,
5.06402871064698));
#6161=CARTESIAN_POINT('Ctrl Pts',(0.825928126169711,-0.996867817321921,
5.06152236891498));
#6162=CARTESIAN_POINT('Ctrl Pts',(0.851027093284864,-0.998125914862946,
5.06152236891498));
#6163=CARTESIAN_POINT('Ctrl Pts',(0.864415297824352,-0.99879518361721,5.06402870334554));
#6164=CARTESIAN_POINT('Ctrl Pts',(0.889053345635921,-0.999738921136592,
5.07423047638114));
#6165=CARTESIAN_POINT('Ctrl Pts',(0.90030335837337,-1.,5.08192673996601));
#6166=CARTESIAN_POINT('Ctrl Pts',(0.909188309203679,-1.,5.09081169079632));
#6167=CARTESIAN_POINT('Ctrl Pts',(0.909188309203679,-1.,5.09081169079632));
#6168=CARTESIAN_POINT('Ctrl Pts',(0.918073260033988,-1.,5.09969664162663));
#6169=CARTESIAN_POINT('Ctrl Pts',(0.925769523618861,-0.999738921136592,
5.11094665436408));
#6170=CARTESIAN_POINT('Ctrl Pts',(0.935971296654457,-0.99879518361721,5.13558470217565));
#6171=CARTESIAN_POINT('Ctrl Pts',(0.938477631085024,-0.998125914862946,
5.14897290671514));
#6172=CARTESIAN_POINT('Ctrl Pts',(0.938477631085024,-0.996867817321921,
5.17407187383029));
#6173=CARTESIAN_POINT('Ctrl Pts',(0.935971289353023,-0.996197082307396,
5.18746005234032));
#6174=CARTESIAN_POINT('Ctrl Pts',(0.925769535239926,-0.995249987974195,
5.21209805634762));
#6175=CARTESIAN_POINT('Ctrl Pts',(0.91807329027631,-0.99498743710662,5.223348065961));
#6176=CARTESIAN_POINT('Ctrl Pts',(0.909188309203679,-0.99498743710662,5.23223304703363));
#6177=CARTESIAN_POINT('Origin',(0.838477631085024,-1.2,5.16152236891498));
#6178=CARTESIAN_POINT('',(0.909188309203679,0.99498743710662,5.23223304703363));
#6179=CARTESIAN_POINT('',(0.909188309203679,1.,5.09081169079632));
#6180=CARTESIAN_POINT('Ctrl Pts',(0.909188309203678,0.99498743710662,5.23223304703363));
#6181=CARTESIAN_POINT('Ctrl Pts',(0.91807329027631,0.99498743710662,5.223348065961));
#6182=CARTESIAN_POINT('Ctrl Pts',(0.925769535239926,0.995249987974195,5.21209805634762));
#6183=CARTESIAN_POINT('Ctrl Pts',(0.935971289353023,0.996197082307397,5.18746005234032));
#6184=CARTESIAN_POINT('Ctrl Pts',(0.938477631085024,0.996867817321921,5.17407187383029));
#6185=CARTESIAN_POINT('Ctrl Pts',(0.938477631085024,0.998125914862946,5.14897290671514));
#6186=CARTESIAN_POINT('Ctrl Pts',(0.935971296654456,0.99879518361721,5.13558470217565));
#6187=CARTESIAN_POINT('Ctrl Pts',(0.925769523618861,0.999738921136592,5.11094665436408));
#6188=CARTESIAN_POINT('Ctrl Pts',(0.918073260033988,1.,5.09969664162663));
#6189=CARTESIAN_POINT('Ctrl Pts',(0.909188309203679,1.,5.09081169079632));
#6190=CARTESIAN_POINT('Ctrl Pts',(0.909188309203679,1.,5.09081169079632));
#6191=CARTESIAN_POINT('Ctrl Pts',(0.900303358373369,1.,5.08192673996601));
#6192=CARTESIAN_POINT('Ctrl Pts',(0.889053345635921,0.999738921136592,5.07423047638114));
#6193=CARTESIAN_POINT('Ctrl Pts',(0.864415297824351,0.99879518361721,5.06402870334554));
#6194=CARTESIAN_POINT('Ctrl Pts',(0.851027093284864,0.998125914862946,5.06152236891498));
#6195=CARTESIAN_POINT('Ctrl Pts',(0.825928126169711,0.996867817321921,5.06152236891498));
#6196=CARTESIAN_POINT('Ctrl Pts',(0.812539947659677,0.996197082307397,5.06402871064698));
#6197=CARTESIAN_POINT('Ctrl Pts',(0.787901943652379,0.995249987974195,5.07423046476007));
#6198=CARTESIAN_POINT('Ctrl Pts',(0.776651934039,0.99498743710662,5.08192670972369));
#6199=CARTESIAN_POINT('Ctrl Pts',(0.758881971893738,0.99498743710662,5.09969667186895));
#6200=CARTESIAN_POINT('Ctrl Pts',(0.751185726930123,0.995249987974195,5.11094668148233));
#6201=CARTESIAN_POINT('Ctrl Pts',(0.740983972817025,0.996197082307397,5.13558468548963));
#6202=CARTESIAN_POINT('Ctrl Pts',(0.738477631085024,0.996867817321921,5.14897286399966));
#6203=CARTESIAN_POINT('Ctrl Pts',(0.738477631085024,0.998125914862946,5.17407183111482));
#6204=CARTESIAN_POINT('Ctrl Pts',(0.740983965515591,0.99879518361721,5.1874600356543));
#6205=CARTESIAN_POINT('Ctrl Pts',(0.751185738551187,0.999738921136592,5.21209808346587));
#6206=CARTESIAN_POINT('Ctrl Pts',(0.75888200213606,1.,5.22334809620332));
#6207=CARTESIAN_POINT('Ctrl Pts',(0.776651903796679,1.,5.24111799786394));
#6208=CARTESIAN_POINT('Ctrl Pts',(0.787901916534127,0.999738921136592,5.24881426144881));
#6209=CARTESIAN_POINT('Ctrl Pts',(0.812539964345696,0.99879518361721,5.25901603448441));
#6210=CARTESIAN_POINT('Ctrl Pts',(0.825928168885184,0.998125914862946,5.26152236891498));
#6211=CARTESIAN_POINT('Ctrl Pts',(0.851027136000337,0.996867817321921,5.26152236891498));
#6212=CARTESIAN_POINT('Ctrl Pts',(0.86441531451037,0.996197082307397,5.25901602718297));
#6213=CARTESIAN_POINT('Ctrl Pts',(0.889053318517669,0.995249987974195,5.24881427306988));
#6214=CARTESIAN_POINT('Ctrl Pts',(0.900303328131047,0.99498743710662,5.24111802810626));
#6215=CARTESIAN_POINT('Ctrl Pts',(0.909188309203679,0.99498743710662,5.23223304703363));
#6216=CARTESIAN_POINT('',(0.909188309203679,1.1,5.09081169079632));
#6217=CARTESIAN_POINT('',(0.909188309203679,-1.2,5.09081169079632));
#6218=CARTESIAN_POINT('',(0.909188309203679,1.09544511501033,5.23223304703363));
#6219=CARTESIAN_POINT('Ctrl Pts',(0.909188309203678,1.09544511501033,5.23223304703363));
#6220=CARTESIAN_POINT('Ctrl Pts',(0.900304443829673,1.09544511501033,5.24111691240764));
#6221=CARTESIAN_POINT('Ctrl Pts',(0.88905534398189,1.09568352051035,5.24881311743569));
#6222=CARTESIAN_POINT('Ctrl Pts',(0.86441734802691,1.09654384276605,5.25901550208007));
#6223=CARTESIAN_POINT('Ctrl Pts',(0.851028301361521,1.09715325263881,5.26152236891498));
#6224=CARTESIAN_POINT('Ctrl Pts',(0.825926989938962,1.09829658604435,5.26152236891498));
#6225=CARTESIAN_POINT('Ctrl Pts',(0.812537925529285,1.09890489533505,5.25901550700422));
#6226=CARTESIAN_POINT('Ctrl Pts',(0.787899899662102,1.09976269863984,5.24881310955496));
#6227=CARTESIAN_POINT('Ctrl Pts',(0.77665079772069,1.1,5.24111689178795));
#6228=CARTESIAN_POINT('Ctrl Pts',(0.758883108212048,1.1,5.22334920227931));
#6229=CARTESIAN_POINT('Ctrl Pts',(0.751186890445044,1.09976269863984,5.2121001003379));
#6230=CARTESIAN_POINT('Ctrl Pts',(0.740984492995779,1.09890489533505,5.18746207447071));
#6231=CARTESIAN_POINT('Ctrl Pts',(0.738477631085024,1.09829658604435,5.17407301006104));
#6232=CARTESIAN_POINT('Ctrl Pts',(0.738477631085024,1.09715325263881,5.14897169863848));
#6233=CARTESIAN_POINT('Ctrl Pts',(0.740984497919934,1.09654384276605,5.13558265197309));
#6234=CARTESIAN_POINT('Ctrl Pts',(0.751186882564314,1.09568352051035,5.11094465601811));
#6235=CARTESIAN_POINT('Ctrl Pts',(0.758883087592363,1.09544511501033,5.09969555617033));
#6236=CARTESIAN_POINT('Ctrl Pts',(0.776650818340375,1.09544511501033,5.08192782542232));
#6237=CARTESIAN_POINT('Ctrl Pts',(0.787899918188158,1.09568352051035,5.07423162039427));
#6238=CARTESIAN_POINT('Ctrl Pts',(0.812537914143137,1.09654384276605,5.06402923574989));
#6239=CARTESIAN_POINT('Ctrl Pts',(0.825926960808527,1.09715325263881,5.06152236891498));
#6240=CARTESIAN_POINT('Ctrl Pts',(0.851028272231085,1.09829658604435,5.06152236891498));
#6241=CARTESIAN_POINT('Ctrl Pts',(0.864417336640762,1.09890489533505,5.06402923082573));
#6242=CARTESIAN_POINT('Ctrl Pts',(0.889055362507946,1.09976269863984,5.074231628275));
#6243=CARTESIAN_POINT('Ctrl Pts',(0.900304464449358,1.1,5.081927846042));
#6244=CARTESIAN_POINT('Ctrl Pts',(0.909188309203679,1.1,5.09081169079632));
#6245=CARTESIAN_POINT('Ctrl Pts',(0.909188309203679,1.1,5.09081169079632));
#6246=CARTESIAN_POINT('Ctrl Pts',(0.918072153958,1.1,5.09969553555064));
#6247=CARTESIAN_POINT('Ctrl Pts',(0.925768371725004,1.09976269863984,5.11094463749205));
#6248=CARTESIAN_POINT('Ctrl Pts',(0.935970769174269,1.09890489533505,5.13558266335924));
#6249=CARTESIAN_POINT('Ctrl Pts',(0.938477631085024,1.09829658604435,5.14897172776891));
#6250=CARTESIAN_POINT('Ctrl Pts',(0.938477631085024,1.09715325263881,5.17407303919147));
#6251=CARTESIAN_POINT('Ctrl Pts',(0.935970764250113,1.09654384276605,5.18746208585686));
#6252=CARTESIAN_POINT('Ctrl Pts',(0.925768379605734,1.09568352051035,5.21210008181184));
#6253=CARTESIAN_POINT('Ctrl Pts',(0.918072174577684,1.09544511501033,5.22334918165963));
#6254=CARTESIAN_POINT('Ctrl Pts',(0.909188309203679,1.09544511501033,5.23223304703363));
#6255=CARTESIAN_POINT('Origin',(0.272792206135786,-1.2,5.72720779386422));
#6256=CARTESIAN_POINT('',(0.343502884254441,-1.09544511501033,5.79791847198287));
#6257=CARTESIAN_POINT('',(0.343502884254441,-1.1,5.65649711574556));
#6258=CARTESIAN_POINT('Ctrl Pts',(0.343502884254441,-1.09544511501033,5.79791847198287));
#6259=CARTESIAN_POINT('Ctrl Pts',(0.352386749628447,-1.09544511501033,5.78903460660886));
#6260=CARTESIAN_POINT('Ctrl Pts',(0.360082954656496,-1.09568352051035,5.77778550676108));
#6261=CARTESIAN_POINT('Ctrl Pts',(0.370285339300875,-1.09654384276605,5.7531475108061));
#6262=CARTESIAN_POINT('Ctrl Pts',(0.372792206135786,-1.09715325263881,5.73975846414071));
#6263=CARTESIAN_POINT('Ctrl Pts',(0.372792206135786,-1.09829658604435,5.71465715271815));
#6264=CARTESIAN_POINT('Ctrl Pts',(0.370285344225031,-1.09890489533505,5.70126808830848));
#6265=CARTESIAN_POINT('Ctrl Pts',(0.360082946775766,-1.09976269863984,5.67663006244129));
#6266=CARTESIAN_POINT('Ctrl Pts',(0.352386729008762,-1.1,5.66538096049988));
#6267=CARTESIAN_POINT('Ctrl Pts',(0.343502884254441,-1.1,5.65649711574556));
#6268=CARTESIAN_POINT('Ctrl Pts',(0.343502884254441,-1.1,5.65649711574556));
#6269=CARTESIAN_POINT('Ctrl Pts',(0.33461903950012,-1.1,5.64761327099124));
#6270=CARTESIAN_POINT('Ctrl Pts',(0.323369937558708,-1.09976269863984,5.63991705322424));
#6271=CARTESIAN_POINT('Ctrl Pts',(0.298731911691524,-1.09890489533505,5.62971465577497));
#6272=CARTESIAN_POINT('Ctrl Pts',(0.285342847281848,-1.09829658604435,5.62720779386421));
#6273=CARTESIAN_POINT('Ctrl Pts',(0.260241535859289,-1.09715325263881,5.62720779386421));
#6274=CARTESIAN_POINT('Ctrl Pts',(0.246852489193899,-1.09654384276605,5.62971466069913));
#6275=CARTESIAN_POINT('Ctrl Pts',(0.22221449323892,-1.09568352051035,5.6399170453435));
#6276=CARTESIAN_POINT('Ctrl Pts',(0.210965393391137,-1.09544511501033,5.64761325037155));
#6277=CARTESIAN_POINT('Ctrl Pts',(0.193197662643126,-1.09544511501033,5.66538098111957));
#6278=CARTESIAN_POINT('Ctrl Pts',(0.185501457615076,-1.09568352051035,5.67663008096735));
#6279=CARTESIAN_POINT('Ctrl Pts',(0.175299072970697,-1.09654384276605,5.70126807692233));
#6280=CARTESIAN_POINT('Ctrl Pts',(0.172792206135786,-1.09715325263881,5.71465712358772));
#6281=CARTESIAN_POINT('Ctrl Pts',(0.172792206135786,-1.09829658604435,5.73975843501028));
#6282=CARTESIAN_POINT('Ctrl Pts',(0.175299068046541,-1.09890489533505,5.75314749941995));
#6283=CARTESIAN_POINT('Ctrl Pts',(0.185501465495806,-1.09976269863984,5.77778552528714));
#6284=CARTESIAN_POINT('Ctrl Pts',(0.19319768326281,-1.1,5.78903462722855));
#6285=CARTESIAN_POINT('Ctrl Pts',(0.210965372771452,-1.1,5.80680231673719));
#6286=CARTESIAN_POINT('Ctrl Pts',(0.222214474712864,-1.09976269863984,5.81449853450419));
#6287=CARTESIAN_POINT('Ctrl Pts',(0.246852500580048,-1.09890489533505,5.82470093195346));
#6288=CARTESIAN_POINT('Ctrl Pts',(0.260241564989724,-1.09829658604435,5.82720779386421));
#6289=CARTESIAN_POINT('Ctrl Pts',(0.285342876412283,-1.09715325263881,5.82720779386421));
#6290=CARTESIAN_POINT('Ctrl Pts',(0.298731923077673,-1.09654384276605,5.8247009270293));
#6291=CARTESIAN_POINT('Ctrl Pts',(0.323369919032652,-1.09568352051035,5.81449854238492));
#6292=CARTESIAN_POINT('Ctrl Pts',(0.334619018880435,-1.09544511501033,5.80680233735688));
#6293=CARTESIAN_POINT('Ctrl Pts',(0.343502884254441,-1.09544511501033,5.79791847198287));
#6294=CARTESIAN_POINT('',(0.343502884254441,-1.,5.65649711574556));
#6295=CARTESIAN_POINT('',(0.343502884254441,-1.2,5.65649711574556));
#6296=CARTESIAN_POINT('',(0.343502884254441,-0.99498743710662,5.79791847198287));
#6297=CARTESIAN_POINT('Ctrl Pts',(0.343502884254441,-0.99498743710662,5.79791847198287));
#6298=CARTESIAN_POINT('Ctrl Pts',(0.33461790318181,-0.99498743710662,5.8068034530555));
#6299=CARTESIAN_POINT('Ctrl Pts',(0.32336789356843,-0.995249987974195,5.81449969801912));
#6300=CARTESIAN_POINT('Ctrl Pts',(0.298729889561132,-0.996197082307397,
5.82470145213221));
#6301=CARTESIAN_POINT('Ctrl Pts',(0.285341711051099,-0.996867817321921,
5.82720779386421));
#6302=CARTESIAN_POINT('Ctrl Pts',(0.260242743935946,-0.998125914862946,
5.82720779386421));
#6303=CARTESIAN_POINT('Ctrl Pts',(0.246854539396459,-0.99879518361721,5.82470145943365));
#6304=CARTESIAN_POINT('Ctrl Pts',(0.222216491584889,-0.999738921136592,
5.81449968639805));
#6305=CARTESIAN_POINT('Ctrl Pts',(0.210966478847441,-1.,5.80680342281318));
#6306=CARTESIAN_POINT('Ctrl Pts',(0.193196577186822,-1.,5.78903352115256));
#6307=CARTESIAN_POINT('Ctrl Pts',(0.185500313601949,-0.999738921136592,
5.77778350841511));
#6308=CARTESIAN_POINT('Ctrl Pts',(0.175298540566354,-0.99879518361721,5.75314546060354));
#6309=CARTESIAN_POINT('Ctrl Pts',(0.172792206135786,-0.998125914862946,
5.73975725606406));
#6310=CARTESIAN_POINT('Ctrl Pts',(0.172792206135786,-0.996867817321921,
5.7146582889489));
#6311=CARTESIAN_POINT('Ctrl Pts',(0.175298547867787,-0.996197082307396,
5.70127011043887));
#6312=CARTESIAN_POINT('Ctrl Pts',(0.185500301980885,-0.995249987974195,
5.67663210643157));
#6313=CARTESIAN_POINT('Ctrl Pts',(0.1931965469445,-0.99498743710662,5.66538209681819));
#6314=CARTESIAN_POINT('Ctrl Pts',(0.210966509089762,-0.99498743710662,5.64761213467293));
#6315=CARTESIAN_POINT('Ctrl Pts',(0.222216518703142,-0.995249987974195,
5.63991588970931));
#6316=CARTESIAN_POINT('Ctrl Pts',(0.24685452271044,-0.996197082307396,5.62971413559622));
#6317=CARTESIAN_POINT('Ctrl Pts',(0.260242701220473,-0.996867817321921,
5.62720779386421));
#6318=CARTESIAN_POINT('Ctrl Pts',(0.285341668335626,-0.998125914862946,
5.62720779386421));
#6319=CARTESIAN_POINT('Ctrl Pts',(0.298729872875113,-0.99879518361721,5.62971412829478));
#6320=CARTESIAN_POINT('Ctrl Pts',(0.323367920686683,-0.999738921136592,
5.63991590133038));
#6321=CARTESIAN_POINT('Ctrl Pts',(0.334617933424131,-1.,5.64761216491525));
#6322=CARTESIAN_POINT('Ctrl Pts',(0.34350288425444,-1.,5.65649711574556));
#6323=CARTESIAN_POINT('Ctrl Pts',(0.343502884254441,-1.,5.65649711574556));
#6324=CARTESIAN_POINT('Ctrl Pts',(0.35238783508475,-1.,5.66538206657587));
#6325=CARTESIAN_POINT('Ctrl Pts',(0.360084098669623,-0.999738921136592,
5.67663207931332));
#6326=CARTESIAN_POINT('Ctrl Pts',(0.370285871705218,-0.99879518361721,5.70127012712489));
#6327=CARTESIAN_POINT('Ctrl Pts',(0.372792206135786,-0.998125914862946,
5.71465833166437));
#6328=CARTESIAN_POINT('Ctrl Pts',(0.372792206135786,-0.996867817321921,
5.73975729877953));
#6329=CARTESIAN_POINT('Ctrl Pts',(0.370285864403785,-0.996197082307397,
5.75314547728956));
#6330=CARTESIAN_POINT('Ctrl Pts',(0.360084110290687,-0.995249987974195,
5.77778348129686));
#6331=CARTESIAN_POINT('Ctrl Pts',(0.352387865327073,-0.99498743710662,5.78903349091024));
#6332=CARTESIAN_POINT('Ctrl Pts',(0.343502884254441,-0.99498743710662,5.79791847198287));
#6333=CARTESIAN_POINT('Origin',(0.272792206135786,-1.2,5.72720779386422));
#6334=CARTESIAN_POINT('',(0.34350288425444,0.99498743710662,5.79791847198287));
#6335=CARTESIAN_POINT('',(0.34350288425444,1.,5.65649711574556));
#6336=CARTESIAN_POINT('Ctrl Pts',(0.343502884254441,0.99498743710662,5.79791847198287));
#6337=CARTESIAN_POINT('Ctrl Pts',(0.352387865327072,0.99498743710662,5.78903349091024));
#6338=CARTESIAN_POINT('Ctrl Pts',(0.360084110290687,0.995249987974195,5.77778348129686));
#6339=CARTESIAN_POINT('Ctrl Pts',(0.370285864403785,0.996197082307397,5.75314547728956));
#6340=CARTESIAN_POINT('Ctrl Pts',(0.372792206135786,0.996867817321921,5.73975729877953));
#6341=CARTESIAN_POINT('Ctrl Pts',(0.372792206135786,0.998125914862946,5.71465833166437));
#6342=CARTESIAN_POINT('Ctrl Pts',(0.370285871705218,0.99879518361721,5.70127012712489));
#6343=CARTESIAN_POINT('Ctrl Pts',(0.360084098669623,0.999738921136592,5.67663207931332));
#6344=CARTESIAN_POINT('Ctrl Pts',(0.35238783508475,1.,5.66538206657587));
#6345=CARTESIAN_POINT('Ctrl Pts',(0.34350288425444,1.,5.65649711574556));
#6346=CARTESIAN_POINT('Ctrl Pts',(0.34350288425444,1.,5.65649711574556));
#6347=CARTESIAN_POINT('Ctrl Pts',(0.334617933424131,1.,5.64761216491525));
#6348=CARTESIAN_POINT('Ctrl Pts',(0.323367920686683,0.999738921136592,5.63991590133038));
#6349=CARTESIAN_POINT('Ctrl Pts',(0.298729872875113,0.99879518361721,5.62971412829478));
#6350=CARTESIAN_POINT('Ctrl Pts',(0.285341668335626,0.998125914862946,5.62720779386421));
#6351=CARTESIAN_POINT('Ctrl Pts',(0.260242701220473,0.996867817321921,5.62720779386421));
#6352=CARTESIAN_POINT('Ctrl Pts',(0.24685452271044,0.996197082307397,5.62971413559622));
#6353=CARTESIAN_POINT('Ctrl Pts',(0.222216518703141,0.995249987974195,5.63991588970931));
#6354=CARTESIAN_POINT('Ctrl Pts',(0.210966509089762,0.99498743710662,5.64761213467293));
#6355=CARTESIAN_POINT('Ctrl Pts',(0.1931965469445,0.99498743710662,5.66538209681819));
#6356=CARTESIAN_POINT('Ctrl Pts',(0.185500301980885,0.995249987974195,5.67663210643157));
#6357=CARTESIAN_POINT('Ctrl Pts',(0.175298547867787,0.996197082307397,5.70127011043887));
#6358=CARTESIAN_POINT('Ctrl Pts',(0.172792206135785,0.996867817321921,5.7146582889489));
#6359=CARTESIAN_POINT('Ctrl Pts',(0.172792206135786,0.998125914862946,5.73975725606405));
#6360=CARTESIAN_POINT('Ctrl Pts',(0.175298540566354,0.99879518361721,5.75314546060354));
#6361=CARTESIAN_POINT('Ctrl Pts',(0.185500313601948,0.999738921136592,5.77778350841511));
#6362=CARTESIAN_POINT('Ctrl Pts',(0.193196577186822,1.,5.78903352115256));
#6363=CARTESIAN_POINT('Ctrl Pts',(0.21096647884744,1.,5.80680342281318));
#6364=CARTESIAN_POINT('Ctrl Pts',(0.222216491584889,0.999738921136592,5.81449968639805));
#6365=CARTESIAN_POINT('Ctrl Pts',(0.246854539396459,0.99879518361721,5.82470145943365));
#6366=CARTESIAN_POINT('Ctrl Pts',(0.260242743935945,0.998125914862946,5.82720779386421));
#6367=CARTESIAN_POINT('Ctrl Pts',(0.285341711051099,0.996867817321921,5.82720779386421));
#6368=CARTESIAN_POINT('Ctrl Pts',(0.298729889561132,0.996197082307397,5.82470145213221));
#6369=CARTESIAN_POINT('Ctrl Pts',(0.32336789356843,0.995249987974195,5.81449969801912));
#6370=CARTESIAN_POINT('Ctrl Pts',(0.33461790318181,0.99498743710662,5.8068034530555));
#6371=CARTESIAN_POINT('Ctrl Pts',(0.343502884254442,0.99498743710662,5.79791847198287));
#6372=CARTESIAN_POINT('',(0.343502884254441,1.1,5.65649711574556));
#6373=CARTESIAN_POINT('',(0.343502884254441,-1.2,5.65649711574556));
#6374=CARTESIAN_POINT('',(0.343502884254441,1.09544511501033,5.79791847198287));
#6375=CARTESIAN_POINT('Ctrl Pts',(0.343502884254441,1.09544511501033,5.79791847198287));
#6376=CARTESIAN_POINT('Ctrl Pts',(0.334619018880436,1.09544511501033,5.80680233735688));
#6377=CARTESIAN_POINT('Ctrl Pts',(0.323369919032652,1.09568352051035,5.81449854238492));
#6378=CARTESIAN_POINT('Ctrl Pts',(0.298731923077672,1.09654384276605,5.8247009270293));
#6379=CARTESIAN_POINT('Ctrl Pts',(0.285342876412283,1.09715325263881,5.82720779386421));
#6380=CARTESIAN_POINT('Ctrl Pts',(0.260241564989724,1.09829658604435,5.82720779386421));
#6381=CARTESIAN_POINT('Ctrl Pts',(0.246852500580047,1.09890489533505,5.82470093195346));
#6382=CARTESIAN_POINT('Ctrl Pts',(0.222214474712864,1.09976269863984,5.81449853450419));
#6383=CARTESIAN_POINT('Ctrl Pts',(0.210965372771452,1.1,5.80680231673719));
#6384=CARTESIAN_POINT('Ctrl Pts',(0.19319768326281,1.1,5.78903462722855));
#6385=CARTESIAN_POINT('Ctrl Pts',(0.185501465495806,1.09976269863984,5.77778552528714));
#6386=CARTESIAN_POINT('Ctrl Pts',(0.17529906804654,1.09890489533505,5.75314749941995));
#6387=CARTESIAN_POINT('Ctrl Pts',(0.172792206135785,1.09829658604435,5.73975843501028));
#6388=CARTESIAN_POINT('Ctrl Pts',(0.172792206135786,1.09715325263881,5.71465712358772));
#6389=CARTESIAN_POINT('Ctrl Pts',(0.175299072970696,1.09654384276605,5.70126807692233));
#6390=CARTESIAN_POINT('Ctrl Pts',(0.185501457615076,1.09568352051035,5.67663008096735));
#6391=CARTESIAN_POINT('Ctrl Pts',(0.193197662643125,1.09544511501033,5.66538098111957));
#6392=CARTESIAN_POINT('Ctrl Pts',(0.210965393391136,1.09544511501033,5.64761325037155));
#6393=CARTESIAN_POINT('Ctrl Pts',(0.22221449323892,1.09568352051035,5.6399170453435));
#6394=CARTESIAN_POINT('Ctrl Pts',(0.246852489193899,1.09654384276605,5.62971466069913));
#6395=CARTESIAN_POINT('Ctrl Pts',(0.260241535859289,1.09715325263881,5.62720779386421));
#6396=CARTESIAN_POINT('Ctrl Pts',(0.285342847281847,1.09829658604435,5.62720779386421));
#6397=CARTESIAN_POINT('Ctrl Pts',(0.298731911691524,1.09890489533505,5.62971465577497));
#6398=CARTESIAN_POINT('Ctrl Pts',(0.323369937558707,1.09976269863984,5.63991705322423));
#6399=CARTESIAN_POINT('Ctrl Pts',(0.334619039500119,1.1,5.64761327099124));
#6400=CARTESIAN_POINT('Ctrl Pts',(0.34350288425444,1.1,5.65649711574556));
#6401=CARTESIAN_POINT('Ctrl Pts',(0.34350288425444,1.1,5.65649711574556));
#6402=CARTESIAN_POINT('Ctrl Pts',(0.352386729008762,1.1,5.66538096049988));
#6403=CARTESIAN_POINT('Ctrl Pts',(0.360082946775765,1.09976269863984,5.67663006244129));
#6404=CARTESIAN_POINT('Ctrl Pts',(0.370285344225031,1.09890489533505,5.70126808830848));
#6405=CARTESIAN_POINT('Ctrl Pts',(0.372792206135786,1.09829658604435,5.71465715271815));
#6406=CARTESIAN_POINT('Ctrl Pts',(0.372792206135786,1.09715325263881,5.73975846414071));
#6407=CARTESIAN_POINT('Ctrl Pts',(0.370285339300875,1.09654384276605,5.7531475108061));
#6408=CARTESIAN_POINT('Ctrl Pts',(0.360082954656496,1.09568352051035,5.77778550676108));
#6409=CARTESIAN_POINT('Ctrl Pts',(0.352386749628446,1.09544511501033,5.78903460660886));
#6410=CARTESIAN_POINT('Ctrl Pts',(0.343502884254441,1.09544511501033,5.79791847198287));
#6411=CARTESIAN_POINT('Origin',(2.53553390593274,-1.2,3.46446609406726));
#6412=CARTESIAN_POINT('',(2.60624458405139,-1.09544511501033,3.53517677218592));
#6413=CARTESIAN_POINT('',(2.60624458405139,-1.1,3.39375541594861));
#6414=CARTESIAN_POINT('Ctrl Pts',(2.60624458405139,-1.09544511501033,3.53517677218592));
#6415=CARTESIAN_POINT('Ctrl Pts',(2.6151284494254,-1.09544511501033,3.52629290681191));
#6416=CARTESIAN_POINT('Ctrl Pts',(2.62282465445345,-1.09568352051035,3.51504380696413));
#6417=CARTESIAN_POINT('Ctrl Pts',(2.63302703909783,-1.09654384276605,3.49040581100915));
#6418=CARTESIAN_POINT('Ctrl Pts',(2.63553390593274,-1.09715325263881,3.47701676434376));
#6419=CARTESIAN_POINT('Ctrl Pts',(2.63553390593274,-1.09829658604435,3.4519154529212));
#6420=CARTESIAN_POINT('Ctrl Pts',(2.63302704402198,-1.09890489533505,3.43852638851152));
#6421=CARTESIAN_POINT('Ctrl Pts',(2.62282464657272,-1.09976269863984,3.41388836264434));
#6422=CARTESIAN_POINT('Ctrl Pts',(2.61512842880571,-1.1,3.40263926070293));
#6423=CARTESIAN_POINT('Ctrl Pts',(2.60624458405139,-1.1,3.39375541594861));
#6424=CARTESIAN_POINT('Ctrl Pts',(2.60624458405139,-1.1,3.39375541594861));
#6425=CARTESIAN_POINT('Ctrl Pts',(2.59736073929707,-1.1,3.38487157119429));
#6426=CARTESIAN_POINT('Ctrl Pts',(2.58611163735566,-1.09976269863984,3.37717535342728));
#6427=CARTESIAN_POINT('Ctrl Pts',(2.56147361148848,-1.09890489533505,3.36697295597802));
#6428=CARTESIAN_POINT('Ctrl Pts',(2.5480845470788,-1.09829658604435,3.36446609406726));
#6429=CARTESIAN_POINT('Ctrl Pts',(2.52298323565624,-1.09715325263881,3.36446609406726));
#6430=CARTESIAN_POINT('Ctrl Pts',(2.50959418899085,-1.09654384276605,3.36697296090217));
#6431=CARTESIAN_POINT('Ctrl Pts',(2.48495619303587,-1.09568352051035,3.37717534554655));
#6432=CARTESIAN_POINT('Ctrl Pts',(2.47370709318809,-1.09544511501033,3.3848715505746));
#6433=CARTESIAN_POINT('Ctrl Pts',(2.45593936244008,-1.09544511501033,3.40263928132261));
#6434=CARTESIAN_POINT('Ctrl Pts',(2.44824315741203,-1.09568352051035,3.4138883811704));
#6435=CARTESIAN_POINT('Ctrl Pts',(2.43804077276765,-1.09654384276605,3.43852637712538));
#6436=CARTESIAN_POINT('Ctrl Pts',(2.43553390593274,-1.09715325263881,3.45191542379077));
#6437=CARTESIAN_POINT('Ctrl Pts',(2.43553390593274,-1.09829658604435,3.47701673521332));
#6438=CARTESIAN_POINT('Ctrl Pts',(2.43804076784349,-1.09890489533505,3.490405799623));
#6439=CARTESIAN_POINT('Ctrl Pts',(2.44824316529276,-1.09976269863984,3.51504382549018));
#6440=CARTESIAN_POINT('Ctrl Pts',(2.45593938305976,-1.1,3.5262929274316));
#6441=CARTESIAN_POINT('Ctrl Pts',(2.47370707256841,-1.1,3.54406061694024));
#6442=CARTESIAN_POINT('Ctrl Pts',(2.48495617450982,-1.09976269863984,3.55175683470724));
#6443=CARTESIAN_POINT('Ctrl Pts',(2.509594200377,-1.09890489533505,3.56195923215651));
#6444=CARTESIAN_POINT('Ctrl Pts',(2.52298326478668,-1.09829658604435,3.56446609406726));
#6445=CARTESIAN_POINT('Ctrl Pts',(2.54808457620924,-1.09715325263881,3.56446609406726));
#6446=CARTESIAN_POINT('Ctrl Pts',(2.56147362287462,-1.09654384276605,3.56195922723235));
#6447=CARTESIAN_POINT('Ctrl Pts',(2.5861116188296,-1.09568352051035,3.55175684258797));
#6448=CARTESIAN_POINT('Ctrl Pts',(2.59736071867739,-1.09544511501033,3.54406063755992));
#6449=CARTESIAN_POINT('Ctrl Pts',(2.60624458405139,-1.09544511501033,3.53517677218592));
#6450=CARTESIAN_POINT('',(2.60624458405139,-1.,3.39375541594861));
#6451=CARTESIAN_POINT('',(2.60624458405139,-1.2,3.39375541594861));
#6452=CARTESIAN_POINT('',(2.60624458405139,-0.99498743710662,3.53517677218592));
#6453=CARTESIAN_POINT('Ctrl Pts',(2.60624458405139,-0.99498743710662,3.53517677218592));
#6454=CARTESIAN_POINT('Ctrl Pts',(2.59735960297876,-0.99498743710662,3.54406175325855));
#6455=CARTESIAN_POINT('Ctrl Pts',(2.58610959336538,-0.995249987974195,3.55175799822216));
#6456=CARTESIAN_POINT('Ctrl Pts',(2.56147158935808,-0.996197082307397,3.56195975233526));
#6457=CARTESIAN_POINT('Ctrl Pts',(2.54808341084805,-0.996867817321921,3.56446609406726));
#6458=CARTESIAN_POINT('Ctrl Pts',(2.5229844437329,-0.998125914862946,3.56446609406726));
#6459=CARTESIAN_POINT('Ctrl Pts',(2.50959623919341,-0.99879518361721,3.5619597596367));
#6460=CARTESIAN_POINT('Ctrl Pts',(2.48495819138184,-0.999738921136592,3.5517579866011));
#6461=CARTESIAN_POINT('Ctrl Pts',(2.47370817864439,-1.,3.54406172301623));
#6462=CARTESIAN_POINT('Ctrl Pts',(2.45593827698377,-1.,3.52629182135561));
#6463=CARTESIAN_POINT('Ctrl Pts',(2.4482420133989,-0.999738921136592,3.51504180861816));
#6464=CARTESIAN_POINT('Ctrl Pts',(2.43804024036331,-0.99879518361721,3.49040376080659));
#6465=CARTESIAN_POINT('Ctrl Pts',(2.43553390593274,-0.998125914862946,3.4770155562671));
#6466=CARTESIAN_POINT('Ctrl Pts',(2.43553390593274,-0.996867817321921,3.45191658915195));
#6467=CARTESIAN_POINT('Ctrl Pts',(2.43804024766474,-0.996197082307397,3.43852841064192));
#6468=CARTESIAN_POINT('Ctrl Pts',(2.44824200177784,-0.995249987974195,3.41389040663462));
#6469=CARTESIAN_POINT('Ctrl Pts',(2.45593824674145,-0.99498743710662,3.40264039702124));
#6470=CARTESIAN_POINT('Ctrl Pts',(2.47370820888672,-0.99498743710662,3.38487043487598));
#6471=CARTESIAN_POINT('Ctrl Pts',(2.48495821850009,-0.995249987974195,3.37717418991236));
#6472=CARTESIAN_POINT('Ctrl Pts',(2.50959622250739,-0.996197082307397,3.36697243579926));
#6473=CARTESIAN_POINT('Ctrl Pts',(2.52298440101743,-0.996867817321921,3.36446609406726));
#6474=CARTESIAN_POINT('Ctrl Pts',(2.54808336813258,-0.998125914862946,3.36446609406726));
#6475=CARTESIAN_POINT('Ctrl Pts',(2.56147157267207,-0.99879518361721,3.36697242849783));
#6476=CARTESIAN_POINT('Ctrl Pts',(2.58610962048364,-0.999738921136592,3.37717420153343));
#6477=CARTESIAN_POINT('Ctrl Pts',(2.59735963322108,-1.,3.3848704651183));
#6478=CARTESIAN_POINT('Ctrl Pts',(2.60624458405139,-1.,3.39375541594861));
#6479=CARTESIAN_POINT('Ctrl Pts',(2.60624458405139,-1.,3.39375541594861));
#6480=CARTESIAN_POINT('Ctrl Pts',(2.6151295348817,-1.,3.40264036677892));
#6481=CARTESIAN_POINT('Ctrl Pts',(2.62282579846658,-0.999738921136592,3.41389037951637));
#6482=CARTESIAN_POINT('Ctrl Pts',(2.63302757150217,-0.99879518361721,3.43852842732794));
#6483=CARTESIAN_POINT('Ctrl Pts',(2.63553390593274,-0.998125914862946,3.45191663186742));
#6484=CARTESIAN_POINT('Ctrl Pts',(2.63553390593274,-0.996867817321921,3.47701559898258));
#6485=CARTESIAN_POINT('Ctrl Pts',(2.63302756420074,-0.996197082307397,3.49040377749261));
#6486=CARTESIAN_POINT('Ctrl Pts',(2.62282581008764,-0.995249987974195,3.51504178149991));
#6487=CARTESIAN_POINT('Ctrl Pts',(2.61512956512402,-0.99498743710662,3.52629179111329));
#6488=CARTESIAN_POINT('Ctrl Pts',(2.60624458405139,-0.99498743710662,3.53517677218592));
#6489=CARTESIAN_POINT('Origin',(2.53553390593274,-1.2,3.46446609406726));
#6490=CARTESIAN_POINT('',(2.60624458405139,0.99498743710662,3.53517677218592));
#6491=CARTESIAN_POINT('',(2.60624458405139,1.,3.39375541594861));
#6492=CARTESIAN_POINT('Ctrl Pts',(2.60624458405139,0.99498743710662,3.53517677218592));
#6493=CARTESIAN_POINT('Ctrl Pts',(2.61512956512402,0.99498743710662,3.52629179111329));
#6494=CARTESIAN_POINT('Ctrl Pts',(2.62282581008764,0.995249987974195,3.51504178149991));
#6495=CARTESIAN_POINT('Ctrl Pts',(2.63302756420074,0.996197082307397,3.49040377749261));
#6496=CARTESIAN_POINT('Ctrl Pts',(2.63553390593274,0.996867817321921,3.47701559898258));
#6497=CARTESIAN_POINT('Ctrl Pts',(2.63553390593274,0.998125914862946,3.45191663186742));
#6498=CARTESIAN_POINT('Ctrl Pts',(2.63302757150217,0.99879518361721,3.43852842732793));
#6499=CARTESIAN_POINT('Ctrl Pts',(2.62282579846658,0.999738921136592,3.41389037951637));
#6500=CARTESIAN_POINT('Ctrl Pts',(2.6151295348817,1.,3.40264036677892));
#6501=CARTESIAN_POINT('Ctrl Pts',(2.60624458405139,1.,3.39375541594861));
#6502=CARTESIAN_POINT('Ctrl Pts',(2.60624458405139,1.,3.39375541594861));
#6503=CARTESIAN_POINT('Ctrl Pts',(2.59735963322108,1.,3.3848704651183));
#6504=CARTESIAN_POINT('Ctrl Pts',(2.58610962048364,0.999738921136592,3.37717420153343));
#6505=CARTESIAN_POINT('Ctrl Pts',(2.56147157267207,0.99879518361721,3.36697242849783));
#6506=CARTESIAN_POINT('Ctrl Pts',(2.54808336813258,0.998125914862946,3.36446609406726));
#6507=CARTESIAN_POINT('Ctrl Pts',(2.52298440101743,0.996867817321921,3.36446609406726));
#6508=CARTESIAN_POINT('Ctrl Pts',(2.50959622250739,0.996197082307397,3.36697243579926));
#6509=CARTESIAN_POINT('Ctrl Pts',(2.4849582185001,0.995249987974195,3.37717418991236));
#6510=CARTESIAN_POINT('Ctrl Pts',(2.47370820888671,0.99498743710662,3.38487043487598));
#6511=CARTESIAN_POINT('Ctrl Pts',(2.45593824674145,0.99498743710662,3.40264039702124));
#6512=CARTESIAN_POINT('Ctrl Pts',(2.44824200177784,0.995249987974195,3.41389040663462));
#6513=CARTESIAN_POINT('Ctrl Pts',(2.43804024766474,0.996197082307397,3.43852841064192));
#6514=CARTESIAN_POINT('Ctrl Pts',(2.43553390593274,0.996867817321921,3.45191658915195));
#6515=CARTESIAN_POINT('Ctrl Pts',(2.43553390593274,0.998125914862946,3.4770155562671));
#6516=CARTESIAN_POINT('Ctrl Pts',(2.43804024036331,0.99879518361721,3.49040376080659));
#6517=CARTESIAN_POINT('Ctrl Pts',(2.4482420133989,0.999738921136592,3.51504180861816));
#6518=CARTESIAN_POINT('Ctrl Pts',(2.45593827698377,1.,3.52629182135561));
#6519=CARTESIAN_POINT('Ctrl Pts',(2.47370817864439,1.,3.54406172301623));
#6520=CARTESIAN_POINT('Ctrl Pts',(2.48495819138184,0.999738921136592,3.5517579866011));
#6521=CARTESIAN_POINT('Ctrl Pts',(2.50959623919341,0.99879518361721,3.56195975963669));
#6522=CARTESIAN_POINT('Ctrl Pts',(2.5229844437329,0.998125914862946,3.56446609406726));
#6523=CARTESIAN_POINT('Ctrl Pts',(2.54808341084805,0.996867817321921,3.56446609406726));
#6524=CARTESIAN_POINT('Ctrl Pts',(2.56147158935808,0.996197082307397,3.56195975233526));
#6525=CARTESIAN_POINT('Ctrl Pts',(2.58610959336538,0.995249987974195,3.55175799822216));
#6526=CARTESIAN_POINT('Ctrl Pts',(2.59735960297876,0.99498743710662,3.54406175325855));
#6527=CARTESIAN_POINT('Ctrl Pts',(2.60624458405139,0.99498743710662,3.53517677218592));
#6528=CARTESIAN_POINT('',(2.60624458405139,1.1,3.39375541594861));
#6529=CARTESIAN_POINT('',(2.60624458405139,-1.2,3.39375541594861));
#6530=CARTESIAN_POINT('',(2.60624458405139,1.09544511501033,3.53517677218592));
#6531=CARTESIAN_POINT('Ctrl Pts',(2.60624458405139,1.09544511501033,3.53517677218592));
#6532=CARTESIAN_POINT('Ctrl Pts',(2.59736071867739,1.09544511501033,3.54406063755992));
#6533=CARTESIAN_POINT('Ctrl Pts',(2.5861116188296,1.09568352051035,3.55175684258797));
#6534=CARTESIAN_POINT('Ctrl Pts',(2.56147362287462,1.09654384276605,3.56195922723235));
#6535=CARTESIAN_POINT('Ctrl Pts',(2.54808457620923,1.09715325263881,3.56446609406726));
#6536=CARTESIAN_POINT('Ctrl Pts',(2.52298326478668,1.09829658604435,3.56446609406726));
#6537=CARTESIAN_POINT('Ctrl Pts',(2.509594200377,1.09890489533505,3.56195923215651));
#6538=CARTESIAN_POINT('Ctrl Pts',(2.48495617450982,1.09976269863984,3.55175683470724));
#6539=CARTESIAN_POINT('Ctrl Pts',(2.4737070725684,1.1,3.54406061694024));
#6540=CARTESIAN_POINT('Ctrl Pts',(2.45593938305976,1.1,3.5262929274316));
#6541=CARTESIAN_POINT('Ctrl Pts',(2.44824316529276,1.09976269863984,3.51504382549018));
#6542=CARTESIAN_POINT('Ctrl Pts',(2.43804076784349,1.09890489533505,3.490405799623));
#6543=CARTESIAN_POINT('Ctrl Pts',(2.43553390593274,1.09829658604435,3.47701673521332));
#6544=CARTESIAN_POINT('Ctrl Pts',(2.43553390593274,1.09715325263881,3.45191542379077));
#6545=CARTESIAN_POINT('Ctrl Pts',(2.43804077276765,1.09654384276605,3.43852637712538));
#6546=CARTESIAN_POINT('Ctrl Pts',(2.44824315741203,1.09568352051035,3.4138883811704));
#6547=CARTESIAN_POINT('Ctrl Pts',(2.45593936244008,1.09544511501033,3.40263928132261));
#6548=CARTESIAN_POINT('Ctrl Pts',(2.47370709318809,1.09544511501033,3.3848715505746));
#6549=CARTESIAN_POINT('Ctrl Pts',(2.48495619303587,1.09568352051035,3.37717534554655));
#6550=CARTESIAN_POINT('Ctrl Pts',(2.50959418899085,1.09654384276605,3.36697296090217));
#6551=CARTESIAN_POINT('Ctrl Pts',(2.52298323565624,1.09715325263881,3.36446609406726));
#6552=CARTESIAN_POINT('Ctrl Pts',(2.5480845470788,1.09829658604435,3.36446609406726));
#6553=CARTESIAN_POINT('Ctrl Pts',(2.56147361148848,1.09890489533505,3.36697295597802));
#6554=CARTESIAN_POINT('Ctrl Pts',(2.58611163735566,1.09976269863984,3.37717535342728));
#6555=CARTESIAN_POINT('Ctrl Pts',(2.59736073929707,1.1,3.38487157119429));
#6556=CARTESIAN_POINT('Ctrl Pts',(2.60624458405139,1.1,3.39375541594861));
#6557=CARTESIAN_POINT('Ctrl Pts',(2.60624458405139,1.1,3.39375541594861));
#6558=CARTESIAN_POINT('Ctrl Pts',(2.61512842880571,1.1,3.40263926070293));
#6559=CARTESIAN_POINT('Ctrl Pts',(2.62282464657272,1.09976269863984,3.41388836264434));
#6560=CARTESIAN_POINT('Ctrl Pts',(2.63302704402198,1.09890489533505,3.43852638851152));
#6561=CARTESIAN_POINT('Ctrl Pts',(2.63553390593274,1.09829658604435,3.4519154529212));
#6562=CARTESIAN_POINT('Ctrl Pts',(2.63553390593274,1.09715325263881,3.47701676434376));
#6563=CARTESIAN_POINT('Ctrl Pts',(2.63302703909783,1.09654384276605,3.49040581100915));
#6564=CARTESIAN_POINT('Ctrl Pts',(2.62282465445345,1.09568352051035,3.51504380696413));
#6565=CARTESIAN_POINT('Ctrl Pts',(2.6151284494254,1.09544511501033,3.52629290681191));
#6566=CARTESIAN_POINT('Ctrl Pts',(2.60624458405139,1.09544511501033,3.53517677218592));
#6567=CARTESIAN_POINT('Origin',(3.70121933088198,-0.848528137423857,3.49878066911802));
#6568=CARTESIAN_POINT('',(3.69894188838714,-0.703885991122829,3.49650322662319));
#6569=CARTESIAN_POINT('',(3.72193000900063,-0.777817459305203,3.37806999099937));
#6570=CARTESIAN_POINT('Ctrl Pts',(3.69894188838714,-0.703885991122829,3.49650322662319));
#6571=CARTESIAN_POINT('Ctrl Pts',(3.70782575376115,-0.703885991122829,3.48761936124919));
#6572=CARTESIAN_POINT('Ctrl Pts',(3.71616147093913,-0.705831016678427,3.47700977355134));
#6573=CARTESIAN_POINT('Ctrl Pts',(3.72890806304252,-0.713657162034742,3.45491598505536));
#6574=CARTESIAN_POINT('Ctrl Pts',(3.73331329315294,-0.719529169803534,3.44342530166548));
#6575=CARTESIAN_POINT('Ctrl Pts',(3.7375609618052,-0.732888284319023,3.42257165889519));
#6576=CARTESIAN_POINT('Ctrl Pts',(3.7376861590528,-0.741266387103756,3.41181465364387));
#6577=CARTESIAN_POINT('Ctrl Pts',(3.73301492512092,-0.759293157295717,3.39270779129407));
#6578=CARTESIAN_POINT('Ctrl Pts',(3.72821183586942,-0.768933614550881,3.38435181786816));
#6579=CARTESIAN_POINT('Ctrl Pts',(3.72193000900063,-0.777817459305202,3.37806999099937));
#6580=CARTESIAN_POINT('Ctrl Pts',(3.72193000900063,-0.777817459305203,3.37806999099937));
#6581=CARTESIAN_POINT('Ctrl Pts',(3.71564818213184,-0.786701304059524,3.37178816413058));
#6582=CARTESIAN_POINT('Ctrl Pts',(3.70705490734577,-0.796006166512776,3.36674777351892));
#6583=CARTESIAN_POINT('Ctrl Pts',(3.68709024169119,-0.812819819637263,3.36121873628225));
#6584=CARTESIAN_POINT('Ctrl Pts',(3.67572492714916,-0.820337643172961,3.36073562423915));
#6585=CARTESIAN_POINT('Ctrl Pts',(3.65372795097333,-0.832079840080031,3.36383995948588));
#6586=CARTESIAN_POINT('Ctrl Pts',(3.64162785771069,-0.837090012141717,3.36763577972354));
#6587=CARTESIAN_POINT('Ctrl Pts',(3.61867374695901,-0.843699478096002,3.37952204957121));
#6588=CARTESIAN_POINT('Ctrl Pts',(3.60782575376115,-0.845307347360138,3.38761936124919));
#6589=CARTESIAN_POINT('Ctrl Pts',(3.59005802301314,-0.845307347360138,3.4053870919972));
#6590=CARTESIAN_POINT('Ctrl Pts',(3.58196071133516,-0.843699478096002,3.41623508519506));
#6591=CARTESIAN_POINT('Ctrl Pts',(3.57007444148749,-0.837090012141717,3.43918919594674));
#6592=CARTESIAN_POINT('Ctrl Pts',(3.56627862124983,-0.832079840080031,3.45128928920938));
#6593=CARTESIAN_POINT('Ctrl Pts',(3.5631742860031,-0.820337643172961,3.47328626538521));
#6594=CARTESIAN_POINT('Ctrl Pts',(3.5636573980462,-0.812819819637263,3.48465157992723));
#6595=CARTESIAN_POINT('Ctrl Pts',(3.56918643528287,-0.796006166512776,3.50461624558182));
#6596=CARTESIAN_POINT('Ctrl Pts',(3.57422682589453,-0.786701304059523,3.51320952036789));
#6597=CARTESIAN_POINT('Ctrl Pts',(3.58679047963211,-0.768933614550882,3.52577317410547));
#6598=CARTESIAN_POINT('Ctrl Pts',(3.59514645305802,-0.759293157295718,3.53057626335697));
#6599=CARTESIAN_POINT('Ctrl Pts',(3.61425331540782,-0.741266387103756,3.53524749728885));
#6600=CARTESIAN_POINT('Ctrl Pts',(3.62501032065914,-0.732888284319023,3.53512230004125));
#6601=CARTESIAN_POINT('Ctrl Pts',(3.64586396342943,-0.719529169803534,3.53087463138898));
#6602=CARTESIAN_POINT('Ctrl Pts',(3.65735464681931,-0.713657162034742,3.52646940127856));
#6603=CARTESIAN_POINT('Ctrl Pts',(3.67944843531529,-0.705831016678427,3.51372280917518));
#6604=CARTESIAN_POINT('Ctrl Pts',(3.69005802301314,-0.703885991122829,3.5053870919972));
#6605=CARTESIAN_POINT('Ctrl Pts',(3.69894188838714,-0.703885991122829,3.49650322662319));
#6606=CARTESIAN_POINT('',(3.67193000900063,-0.707106781186548,3.32806999099937));
#6607=CARTESIAN_POINT('',(3.77193000900063,-0.848528137423857,3.42806999099937));
#6608=CARTESIAN_POINT('',(3.64871304943529,-0.63285168585486,3.44627438767133));
#6609=CARTESIAN_POINT('Ctrl Pts',(3.64871304943529,-0.63285168585486,3.44627438767133));
#6610=CARTESIAN_POINT('Ctrl Pts',(3.63982806836265,-0.63285168585486,3.45515936874397));
#6611=CARTESIAN_POINT('Ctrl Pts',(3.62922977096665,-0.634814219678611,3.46350732592496));
#6612=CARTESIAN_POINT('Ctrl Pts',(3.60717945397551,-0.642702041451141,3.47629676705421));
#6613=CARTESIAN_POINT('Ctrl Pts',(3.595720251073,-0.648617241117307,3.48073208439373));
#6614=CARTESIAN_POINT('Ctrl Pts',(3.57492599136198,-0.662056333977536,3.48503679179787));
#6615=CARTESIAN_POINT('Ctrl Pts',(3.56420012253987,-0.67047684793714,3.48519279308468));
#6616=CARTESIAN_POINT('Ctrl Pts',(3.5451361171234,-0.688564081560337,3.48056506244418));
#6617=CARTESIAN_POINT('Ctrl Pts',(3.53679126174594,-0.698221830356238,3.4757739562193));
#6618=CARTESIAN_POINT('Ctrl Pts',(3.5242260437807,-0.715991732016857,3.46320873825406));
#6619=CARTESIAN_POINT('Ctrl Pts',(3.51917385869241,-0.725280259543277,3.45460280401319));
#6620=CARTESIAN_POINT('Ctrl Pts',(3.51360239053253,-0.742032846767244,3.43459506107734));
#6621=CARTESIAN_POINT('Ctrl Pts',(3.51308912306508,-0.749506871777695,3.42319992350097));
#6622=CARTESIAN_POINT('Ctrl Pts',(3.51613573292819,-0.761166746032619,3.40114756624893));
#6623=CARTESIAN_POINT('Ctrl Pts',(3.51990031525319,-0.766133383144486,3.38901762833189));
#6624=CARTESIAN_POINT('Ctrl Pts',(3.53174266204924,-0.772681811266156,3.36602021700754));
#6625=CARTESIAN_POINT('Ctrl Pts',(3.53982806836266,-0.774273042092169,3.35515936874397));
#6626=CARTESIAN_POINT('Ctrl Pts',(3.55759803050792,-0.774273042092169,3.3373894065987));
#6627=CARTESIAN_POINT('Ctrl Pts',(3.5684588787715,-0.772681811266156,3.32930400028529));
#6628=CARTESIAN_POINT('Ctrl Pts',(3.59145629009584,-0.766133383144486,3.31746165348924));
#6629=CARTESIAN_POINT('Ctrl Pts',(3.60358622801288,-0.761166746032619,3.31369707116424));
#6630=CARTESIAN_POINT('Ctrl Pts',(3.62563858526492,-0.749506871777695,3.31065046130113));
#6631=CARTESIAN_POINT('Ctrl Pts',(3.63703372284129,-0.742032846767245,3.31116372876858));
#6632=CARTESIAN_POINT('Ctrl Pts',(3.65704146577714,-0.725280259543277,3.31673519692846));
#6633=CARTESIAN_POINT('Ctrl Pts',(3.66564740001801,-0.715991732016856,3.32178738201675));
#6634=CARTESIAN_POINT('Ctrl Pts',(3.67193000900063,-0.707106781186547,3.32806999099937));
#6635=CARTESIAN_POINT('Ctrl Pts',(3.67193000900063,-0.707106781186547,3.32806999099937));
#6636=CARTESIAN_POINT('Ctrl Pts',(3.67821261798325,-0.698221830356238,3.33435259998199));
#6637=CARTESIAN_POINT('Ctrl Pts',(3.68300372420813,-0.688564081560337,3.34269745535945));
#6638=CARTESIAN_POINT('Ctrl Pts',(3.68763145484863,-0.67047684793714,3.36176146077592));
#6639=CARTESIAN_POINT('Ctrl Pts',(3.68747545356182,-0.662056333977536,3.37248732959803));
#6640=CARTESIAN_POINT('Ctrl Pts',(3.68317074615768,-0.648617241117307,3.39328158930905));
#6641=CARTESIAN_POINT('Ctrl Pts',(3.67873542881816,-0.642702041451141,3.40474079221156));
#6642=CARTESIAN_POINT('Ctrl Pts',(3.66594598768891,-0.634814219678611,3.4267911092027));
#6643=CARTESIAN_POINT('Ctrl Pts',(3.65759803050792,-0.63285168585486,3.4373894065987));
#6644=CARTESIAN_POINT('Ctrl Pts',(3.64871304943529,-0.63285168585486,3.44627438767133));
#6645=CARTESIAN_POINT('Origin',(3.70121933088198,-0.848528137423857,3.49878066911802));
#6646=CARTESIAN_POINT('',(2.65372561232867,0.774273042092169,2.45128695056471));
#6647=CARTESIAN_POINT('',(2.67193000900063,0.707106781186548,2.32806999099937));
#6648=CARTESIAN_POINT('Ctrl Pts',(2.65372561232867,0.774273042092169,2.45128695056471));
#6649=CARTESIAN_POINT('Ctrl Pts',(2.6626105934013,0.774273042092169,2.44240196949208));
#6650=CARTESIAN_POINT('Ctrl Pts',(2.67069599971471,0.772681811266156,2.4315411212285));
#6651=CARTESIAN_POINT('Ctrl Pts',(2.68253834651076,0.766133383144486,2.40854370990416));
#6652=CARTESIAN_POINT('Ctrl Pts',(2.68630292883576,0.76116674603262,2.39641377198712));
#6653=CARTESIAN_POINT('Ctrl Pts',(2.68934953869888,0.749506871777696,2.37436141473508));
#6654=CARTESIAN_POINT('Ctrl Pts',(2.68883627123142,0.742032846767245,2.36296627715871));
#6655=CARTESIAN_POINT('Ctrl Pts',(2.68326480307154,0.725280259543277,2.34295853422286));
#6656=CARTESIAN_POINT('Ctrl Pts',(2.67821261798325,0.715991732016857,2.33435259998199));
#6657=CARTESIAN_POINT('Ctrl Pts',(2.67193000900063,0.707106781186548,2.32806999099937));
#6658=CARTESIAN_POINT('Ctrl Pts',(2.67193000900063,0.707106781186548,2.32806999099937));
#6659=CARTESIAN_POINT('Ctrl Pts',(2.66564740001801,0.698221830356239,2.32178738201675));
#6660=CARTESIAN_POINT('Ctrl Pts',(2.65730254464055,0.688564081560338,2.31699627579187));
#6661=CARTESIAN_POINT('Ctrl Pts',(2.63823853922408,0.67047684793714,2.31236854515137));
#6662=CARTESIAN_POINT('Ctrl Pts',(2.62751267040197,0.662056333977536,2.31252454643818));
#6663=CARTESIAN_POINT('Ctrl Pts',(2.60671841069096,0.648617241117307,2.31682925384232));
#6664=CARTESIAN_POINT('Ctrl Pts',(2.59525920778845,0.642702041451142,2.32126457118184));
#6665=CARTESIAN_POINT('Ctrl Pts',(2.5732088907973,0.634814219678611,2.33405401231109));
#6666=CARTESIAN_POINT('Ctrl Pts',(2.5626105934013,0.63285168585486,2.34240196949208));
#6667=CARTESIAN_POINT('Ctrl Pts',(2.54484063125604,0.63285168585486,2.36017193163735));
#6668=CARTESIAN_POINT('Ctrl Pts',(2.53649267407505,0.634814219678611,2.37077022903335));
#6669=CARTESIAN_POINT('Ctrl Pts',(2.52370323294579,0.642702041451141,2.39282054602449));
#6670=CARTESIAN_POINT('Ctrl Pts',(2.51926791560627,0.648617241117307,2.404279748927));
#6671=CARTESIAN_POINT('Ctrl Pts',(2.51496320820213,0.662056333977536,2.42507400863802));
#6672=CARTESIAN_POINT('Ctrl Pts',(2.51480720691532,0.67047684793714,2.43579987746013));
#6673=CARTESIAN_POINT('Ctrl Pts',(2.51943493755582,0.688564081560337,2.4548638828766));
#6674=CARTESIAN_POINT('Ctrl Pts',(2.5242260437807,0.698221830356238,2.46320873825406));
#6675=CARTESIAN_POINT('Ctrl Pts',(2.53679126174594,0.715991732016857,2.4757739562193));
#6676=CARTESIAN_POINT('Ctrl Pts',(2.54539719598681,0.725280259543277,2.48082614130759));
#6677=CARTESIAN_POINT('Ctrl Pts',(2.56540493892266,0.742032846767245,2.48639760946747));
#6678=CARTESIAN_POINT('Ctrl Pts',(2.57680007649903,0.749506871777696,2.48691087693492));
#6679=CARTESIAN_POINT('Ctrl Pts',(2.59885243375108,0.76116674603262,2.48386426707181));
#6680=CARTESIAN_POINT('Ctrl Pts',(2.61098237166811,0.766133383144486,2.48009968474681));
#6681=CARTESIAN_POINT('Ctrl Pts',(2.63397978299246,0.772681811266156,2.46825733795076));
#6682=CARTESIAN_POINT('Ctrl Pts',(2.64484063125603,0.774273042092169,2.46017193163735));
#6683=CARTESIAN_POINT('Ctrl Pts',(2.65372561232867,0.774273042092169,2.45128695056471));
#6684=CARTESIAN_POINT('',(2.62193000900063,0.777817459305202,2.27806999099937));
#6685=CARTESIAN_POINT('',(3.77193000900063,-0.848528137423857,3.42806999099937));
#6686=CARTESIAN_POINT('',(2.60349677337681,0.845307347360138,2.40105811161286));
#6687=CARTESIAN_POINT('Ctrl Pts',(2.60349677337681,0.845307347360138,2.40105811161286));
#6688=CARTESIAN_POINT('Ctrl Pts',(2.5946129080028,0.845307347360138,2.40994197698686));
#6689=CARTESIAN_POINT('Ctrl Pts',(2.58376491480494,0.843699478096002,2.41803928866484));
#6690=CARTESIAN_POINT('Ctrl Pts',(2.56081080405326,0.837090012141717,2.42992555851251));
#6691=CARTESIAN_POINT('Ctrl Pts',(2.54871071079062,0.832079840080031,2.43372137875017));
#6692=CARTESIAN_POINT('Ctrl Pts',(2.52671373461479,0.820337643172961,2.4368257139969));
#6693=CARTESIAN_POINT('Ctrl Pts',(2.51534842007277,0.812819819637263,2.4363426019538));
#6694=CARTESIAN_POINT('Ctrl Pts',(2.49538375441818,0.796006166512776,2.43081356471713));
#6695=CARTESIAN_POINT('Ctrl Pts',(2.48679047963211,0.786701304059523,2.42577317410547));
#6696=CARTESIAN_POINT('Ctrl Pts',(2.47422682589453,0.768933614550882,2.41320952036789));
#6697=CARTESIAN_POINT('Ctrl Pts',(2.46942373664303,0.759293157295718,2.40485354694198));
#6698=CARTESIAN_POINT('Ctrl Pts',(2.46475250271115,0.741266387103757,2.38574668459218));
#6699=CARTESIAN_POINT('Ctrl Pts',(2.46487769995875,0.732888284319023,2.37498967934086));
#6700=CARTESIAN_POINT('Ctrl Pts',(2.46912536861102,0.719529169803535,2.35413603657057));
#6701=CARTESIAN_POINT('Ctrl Pts',(2.47353059872144,0.713657162034742,2.34264535318069));
#6702=CARTESIAN_POINT('Ctrl Pts',(2.48627719082482,0.705831016678427,2.32055156468471));
#6703=CARTESIAN_POINT('Ctrl Pts',(2.4946129080028,0.703885991122829,2.30994197698686));
#6704=CARTESIAN_POINT('Ctrl Pts',(2.51238063875082,0.703885991122829,2.29217424623885));
#6705=CARTESIAN_POINT('Ctrl Pts',(2.52299022644867,0.705831016678427,2.28383852906087));
#6706=CARTESIAN_POINT('Ctrl Pts',(2.54508401494464,0.713657162034742,2.27109193695749));
#6707=CARTESIAN_POINT('Ctrl Pts',(2.55657469833452,0.719529169803534,2.26668670684707));
#6708=CARTESIAN_POINT('Ctrl Pts',(2.57742834110482,0.732888284319023,2.2624390381948));
#6709=CARTESIAN_POINT('Ctrl Pts',(2.58818534635613,0.741266387103757,2.2623138409472));
#6710=CARTESIAN_POINT('Ctrl Pts',(2.60729220870594,0.759293157295719,2.26698507487908));
#6711=CARTESIAN_POINT('Ctrl Pts',(2.61564818213184,0.768933614550882,2.27178816413058));
#6712=CARTESIAN_POINT('Ctrl Pts',(2.62193000900063,0.777817459305203,2.27806999099937));
#6713=CARTESIAN_POINT('Ctrl Pts',(2.62193000900063,0.777817459305203,2.27806999099937));
#6714=CARTESIAN_POINT('Ctrl Pts',(2.62821183586942,0.786701304059524,2.28435181786816));
#6715=CARTESIAN_POINT('Ctrl Pts',(2.63325222648108,0.796006166512776,2.29294509265423));
#6716=CARTESIAN_POINT('Ctrl Pts',(2.63878126371775,0.812819819637263,2.31290975830882));
#6717=CARTESIAN_POINT('Ctrl Pts',(2.63926437576085,0.820337643172961,2.32427507285084));
#6718=CARTESIAN_POINT('Ctrl Pts',(2.63616004051412,0.832079840080031,2.34627204902667));
#6719=CARTESIAN_POINT('Ctrl Pts',(2.63236422027647,0.837090012141717,2.35837214228931));
#6720=CARTESIAN_POINT('Ctrl Pts',(2.62047795042879,0.843699478096002,2.38132625304099));
#6721=CARTESIAN_POINT('Ctrl Pts',(2.61238063875082,0.845307347360138,2.39217424623885));
#6722=CARTESIAN_POINT('Ctrl Pts',(2.60349677337681,0.845307347360138,2.40105811161286));
#6723=CARTESIAN_POINT('Origin',(2.5698484809835,-0.848528137423857,4.6301515190165));
#6724=CARTESIAN_POINT('',(2.56757103848867,-0.703885991122829,4.62787407652167));
#6725=CARTESIAN_POINT('',(2.59055915910216,-0.777817459305203,4.50944084089785));
#6726=CARTESIAN_POINT('Ctrl Pts',(2.56757103848867,-0.703885991122829,4.62787407652167));
#6727=CARTESIAN_POINT('Ctrl Pts',(2.57645490386267,-0.703885991122829,4.61899021114766));
#6728=CARTESIAN_POINT('Ctrl Pts',(2.58479062104066,-0.705831016678427,4.60838062344981));
#6729=CARTESIAN_POINT('Ctrl Pts',(2.59753721314404,-0.713657162034742,4.58628683495384));
#6730=CARTESIAN_POINT('Ctrl Pts',(2.60194244325446,-0.719529169803534,4.57479615156396));
#6731=CARTESIAN_POINT('Ctrl Pts',(2.60619011190672,-0.732888284319023,4.55394250879366));
#6732=CARTESIAN_POINT('Ctrl Pts',(2.60631530915433,-0.741266387103756,4.54318550354234));
#6733=CARTESIAN_POINT('Ctrl Pts',(2.60164407522244,-0.759293157295718,4.52407864119254));
#6734=CARTESIAN_POINT('Ctrl Pts',(2.59684098597094,-0.768933614550882,4.51572266776664));
#6735=CARTESIAN_POINT('Ctrl Pts',(2.59055915910216,-0.777817459305203,4.50944084089785));
#6736=CARTESIAN_POINT('Ctrl Pts',(2.59055915910215,-0.777817459305203,4.50944084089785));
#6737=CARTESIAN_POINT('Ctrl Pts',(2.58427733223337,-0.786701304059524,4.50315901402906));
#6738=CARTESIAN_POINT('Ctrl Pts',(2.5756840574473,-0.796006166512776,4.4981186234174));
#6739=CARTESIAN_POINT('Ctrl Pts',(2.55571939179271,-0.812819819637263,4.49258958618073));
#6740=CARTESIAN_POINT('Ctrl Pts',(2.54435407725069,-0.820337643172961,4.49210647413763));
#6741=CARTESIAN_POINT('Ctrl Pts',(2.52235710107486,-0.832079840080031,4.49521080938436));
#6742=CARTESIAN_POINT('Ctrl Pts',(2.51025700781221,-0.837090012141717,4.49900662962201));
#6743=CARTESIAN_POINT('Ctrl Pts',(2.48730289706053,-0.843699478096002,4.51089289946969));
#6744=CARTESIAN_POINT('Ctrl Pts',(2.47645490386267,-0.845307347360138,4.51899021114766));
#6745=CARTESIAN_POINT('Ctrl Pts',(2.45868717311466,-0.845307347360138,4.53675794189567));
#6746=CARTESIAN_POINT('Ctrl Pts',(2.45058986143669,-0.843699478096002,4.54760593509353));
#6747=CARTESIAN_POINT('Ctrl Pts',(2.43870359158901,-0.837090012141717,4.57056004584521));
#6748=CARTESIAN_POINT('Ctrl Pts',(2.43490777135135,-0.832079840080031,4.58266013910786));
#6749=CARTESIAN_POINT('Ctrl Pts',(2.43180343610462,-0.820337643172961,4.60465711528369));
#6750=CARTESIAN_POINT('Ctrl Pts',(2.43228654814773,-0.812819819637263,4.61602242982571));
#6751=CARTESIAN_POINT('Ctrl Pts',(2.4378155853844,-0.796006166512776,4.6359870954803));
#6752=CARTESIAN_POINT('Ctrl Pts',(2.44285597599606,-0.786701304059523,4.64458037026637));
#6753=CARTESIAN_POINT('Ctrl Pts',(2.45541962973363,-0.768933614550882,4.65714402400394));
#6754=CARTESIAN_POINT('Ctrl Pts',(2.46377560315954,-0.759293157295718,4.66194711325544));
#6755=CARTESIAN_POINT('Ctrl Pts',(2.48288246550934,-0.741266387103756,4.66661834718733));
#6756=CARTESIAN_POINT('Ctrl Pts',(2.49363947076066,-0.732888284319023,4.66649314993972));
#6757=CARTESIAN_POINT('Ctrl Pts',(2.51449311353096,-0.719529169803534,4.66224548128746));
#6758=CARTESIAN_POINT('Ctrl Pts',(2.52598379692084,-0.713657162034742,4.65784025117704));
#6759=CARTESIAN_POINT('Ctrl Pts',(2.54807758541681,-0.705831016678427,4.64509365907366));
#6760=CARTESIAN_POINT('Ctrl Pts',(2.55868717311466,-0.703885991122829,4.63675794189567));
#6761=CARTESIAN_POINT('Ctrl Pts',(2.56757103848867,-0.703885991122829,4.62787407652167));
#6762=CARTESIAN_POINT('',(2.54055915910216,-0.707106781186547,4.45944084089785));
#6763=CARTESIAN_POINT('',(2.64055915910216,-0.848528137423857,4.55944084089785));
#6764=CARTESIAN_POINT('',(2.51734219953681,-0.63285168585486,4.57764523756981));
#6765=CARTESIAN_POINT('Ctrl Pts',(2.51734219953681,-0.63285168585486,4.57764523756981));
#6766=CARTESIAN_POINT('Ctrl Pts',(2.50845721846418,-0.63285168585486,4.58653021864244));
#6767=CARTESIAN_POINT('Ctrl Pts',(2.49785892106817,-0.634814219678611,4.59487817582343));
#6768=CARTESIAN_POINT('Ctrl Pts',(2.47580860407703,-0.642702041451141,4.60766761695268));
#6769=CARTESIAN_POINT('Ctrl Pts',(2.46434940117452,-0.648617241117307,4.61210293429221));
#6770=CARTESIAN_POINT('Ctrl Pts',(2.4435551414635,-0.662056333977536,4.61640764169635));
#6771=CARTESIAN_POINT('Ctrl Pts',(2.4328292726414,-0.67047684793714,4.61656364298316));
#6772=CARTESIAN_POINT('Ctrl Pts',(2.41376526722492,-0.688564081560337,4.61193591234266));
#6773=CARTESIAN_POINT('Ctrl Pts',(2.40542041184747,-0.698221830356238,4.60714480611778));
#6774=CARTESIAN_POINT('Ctrl Pts',(2.39285519388222,-0.715991732016857,4.59457958815253));
#6775=CARTESIAN_POINT('Ctrl Pts',(2.38780300879394,-0.725280259543277,4.58597365391167));
#6776=CARTESIAN_POINT('Ctrl Pts',(2.38223154063405,-0.742032846767244,4.56596591097581));
#6777=CARTESIAN_POINT('Ctrl Pts',(2.3817182731666,-0.749506871777695,4.55457077339944));
#6778=CARTESIAN_POINT('Ctrl Pts',(2.38476488302971,-0.761166746032619,4.5325184161474));
#6779=CARTESIAN_POINT('Ctrl Pts',(2.38852946535471,-0.766133383144486,4.52038847823037));
#6780=CARTESIAN_POINT('Ctrl Pts',(2.40037181215076,-0.772681811266156,4.49739106690602));
#6781=CARTESIAN_POINT('Ctrl Pts',(2.40845721846418,-0.774273042092169,4.48653021864244));
#6782=CARTESIAN_POINT('Ctrl Pts',(2.42622718060944,-0.774273042092169,4.46876025649718));
#6783=CARTESIAN_POINT('Ctrl Pts',(2.43708802887302,-0.772681811266156,4.46067485018376));
#6784=CARTESIAN_POINT('Ctrl Pts',(2.46008544019737,-0.766133383144486,4.44883250338771));
#6785=CARTESIAN_POINT('Ctrl Pts',(2.4722153781144,-0.761166746032619,4.44506792106271));
#6786=CARTESIAN_POINT('Ctrl Pts',(2.49426773536644,-0.749506871777695,4.4420213111996));
#6787=CARTESIAN_POINT('Ctrl Pts',(2.50566287294281,-0.742032846767245,4.44253457866705));
#6788=CARTESIAN_POINT('Ctrl Pts',(2.52567061587867,-0.725280259543277,4.44810604682694));
#6789=CARTESIAN_POINT('Ctrl Pts',(2.53427655011953,-0.715991732016857,4.45315823191522));
#6790=CARTESIAN_POINT('Ctrl Pts',(2.54055915910216,-0.707106781186547,4.45944084089785));
#6791=CARTESIAN_POINT('Ctrl Pts',(2.54055915910216,-0.707106781186547,4.45944084089785));
#6792=CARTESIAN_POINT('Ctrl Pts',(2.54684176808478,-0.698221830356238,4.46572344988047));
#6793=CARTESIAN_POINT('Ctrl Pts',(2.55163287430966,-0.688564081560337,4.47406830525792));
#6794=CARTESIAN_POINT('Ctrl Pts',(2.55626060495016,-0.67047684793714,4.4931323106744));
#6795=CARTESIAN_POINT('Ctrl Pts',(2.55610460366334,-0.662056333977536,4.50385817949651));
#6796=CARTESIAN_POINT('Ctrl Pts',(2.55179989625921,-0.648617241117307,4.52465243920752));
#6797=CARTESIAN_POINT('Ctrl Pts',(2.54736457891968,-0.642702041451141,4.53611164211003));
#6798=CARTESIAN_POINT('Ctrl Pts',(2.53457513779043,-0.634814219678611,4.55816195910118));
#6799=CARTESIAN_POINT('Ctrl Pts',(2.52622718060944,-0.63285168585486,4.56876025649718));
#6800=CARTESIAN_POINT('Ctrl Pts',(2.51734219953681,-0.63285168585486,4.57764523756981));
#6801=CARTESIAN_POINT('Origin',(2.5698484809835,-0.848528137423857,4.6301515190165));
#6802=CARTESIAN_POINT('',(1.52235476243019,0.774273042092169,3.58265780046319));
#6803=CARTESIAN_POINT('',(1.54055915910216,0.707106781186548,3.45944084089785));
#6804=CARTESIAN_POINT('Ctrl Pts',(1.52235476243019,0.774273042092169,3.58265780046319));
#6805=CARTESIAN_POINT('Ctrl Pts',(1.53123974350282,0.774273042092169,3.57377281939056));
#6806=CARTESIAN_POINT('Ctrl Pts',(1.53932514981624,0.772681811266156,3.56291197112698));
#6807=CARTESIAN_POINT('Ctrl Pts',(1.55116749661229,0.766133383144486,3.53991455980264));
#6808=CARTESIAN_POINT('Ctrl Pts',(1.55493207893729,0.76116674603262,3.5277846218856));
#6809=CARTESIAN_POINT('Ctrl Pts',(1.5579786888004,0.749506871777696,3.50573226463356));
#6810=CARTESIAN_POINT('Ctrl Pts',(1.55746542133295,0.742032846767245,3.49433712705719));
#6811=CARTESIAN_POINT('Ctrl Pts',(1.55189395317307,0.725280259543277,3.47432938412133));
#6812=CARTESIAN_POINT('Ctrl Pts',(1.54684176808478,0.715991732016857,3.46572344988047));
#6813=CARTESIAN_POINT('Ctrl Pts',(1.54055915910216,0.707106781186547,3.45944084089785));
#6814=CARTESIAN_POINT('Ctrl Pts',(1.54055915910216,0.707106781186548,3.45944084089785));
#6815=CARTESIAN_POINT('Ctrl Pts',(1.53427655011953,0.698221830356238,3.45315823191522));
#6816=CARTESIAN_POINT('Ctrl Pts',(1.52593169474208,0.688564081560338,3.44836712569034));
#6817=CARTESIAN_POINT('Ctrl Pts',(1.5068676893256,0.67047684793714,3.44373939504984));
#6818=CARTESIAN_POINT('Ctrl Pts',(1.4961418205035,0.662056333977536,3.44389539633666));
#6819=CARTESIAN_POINT('Ctrl Pts',(1.47534756079248,0.648617241117307,3.44820010374079));
#6820=CARTESIAN_POINT('Ctrl Pts',(1.46388835788997,0.642702041451141,3.45263542108032));
#6821=CARTESIAN_POINT('Ctrl Pts',(1.44183804089883,0.634814219678611,3.46542486220957));
#6822=CARTESIAN_POINT('Ctrl Pts',(1.43123974350282,0.63285168585486,3.47377281939056));
#6823=CARTESIAN_POINT('Ctrl Pts',(1.41346978135756,0.63285168585486,3.49154278153582));
#6824=CARTESIAN_POINT('Ctrl Pts',(1.40512182417657,0.634814219678611,3.50214107893183));
#6825=CARTESIAN_POINT('Ctrl Pts',(1.39233238304732,0.642702041451141,3.52419139592297));
#6826=CARTESIAN_POINT('Ctrl Pts',(1.38789706570779,0.648617241117307,3.53565059882548));
#6827=CARTESIAN_POINT('Ctrl Pts',(1.38359235830366,0.662056333977536,3.5564448585365));
#6828=CARTESIAN_POINT('Ctrl Pts',(1.38343635701684,0.67047684793714,3.5671707273586));
#6829=CARTESIAN_POINT('Ctrl Pts',(1.38806408765734,0.688564081560337,3.58623473277508));
#6830=CARTESIAN_POINT('Ctrl Pts',(1.39285519388222,0.698221830356238,3.59457958815253));
#6831=CARTESIAN_POINT('Ctrl Pts',(1.40542041184747,0.715991732016857,3.60714480611778));
#6832=CARTESIAN_POINT('Ctrl Pts',(1.41402634608833,0.725280259543277,3.61219699120607));
#6833=CARTESIAN_POINT('Ctrl Pts',(1.43403408902419,0.742032846767245,3.61776845936595));
#6834=CARTESIAN_POINT('Ctrl Pts',(1.44542922660056,0.749506871777696,3.6182817268334));
#6835=CARTESIAN_POINT('Ctrl Pts',(1.4674815838526,0.76116674603262,3.61523511697029));
#6836=CARTESIAN_POINT('Ctrl Pts',(1.47961152176963,0.766133383144486,3.61147053464529));
#6837=CARTESIAN_POINT('Ctrl Pts',(1.50260893309398,0.772681811266156,3.59962818784924));
#6838=CARTESIAN_POINT('Ctrl Pts',(1.51346978135756,0.774273042092169,3.59154278153582));
#6839=CARTESIAN_POINT('Ctrl Pts',(1.52235476243019,0.774273042092169,3.58265780046319));
#6840=CARTESIAN_POINT('',(1.49055915910215,0.777817459305203,3.40944084089785));
#6841=CARTESIAN_POINT('',(2.64055915910216,-0.848528137423857,4.55944084089785));
#6842=CARTESIAN_POINT('',(1.47212592347833,0.845307347360138,3.53242896151133));
#6843=CARTESIAN_POINT('Ctrl Pts',(1.47212592347833,0.845307347360138,3.53242896151133));
#6844=CARTESIAN_POINT('Ctrl Pts',(1.46324205810433,0.845307347360138,3.54131282688534));
#6845=CARTESIAN_POINT('Ctrl Pts',(1.45239406490647,0.843699478096002,3.54941013856331));
#6846=CARTESIAN_POINT('Ctrl Pts',(1.42943995415479,0.837090012141717,3.56129640841099));
#6847=CARTESIAN_POINT('Ctrl Pts',(1.41733986089214,0.832079840080031,3.56509222864865));
#6848=CARTESIAN_POINT('Ctrl Pts',(1.39534288471631,0.820337643172961,3.56819656389538));
#6849=CARTESIAN_POINT('Ctrl Pts',(1.38397757017429,0.812819819637263,3.56771345185227));
#6850=CARTESIAN_POINT('Ctrl Pts',(1.3640129045197,0.796006166512776,3.5621844146156));
#6851=CARTESIAN_POINT('Ctrl Pts',(1.35541962973363,0.786701304059523,3.55714402400394));
#6852=CARTESIAN_POINT('Ctrl Pts',(1.34285597599606,0.768933614550882,3.54458037026637));
#6853=CARTESIAN_POINT('Ctrl Pts',(1.33805288674456,0.759293157295718,3.53622439684046));
#6854=CARTESIAN_POINT('Ctrl Pts',(1.33338165281267,0.741266387103757,3.51711753449066));
#6855=CARTESIAN_POINT('Ctrl Pts',(1.33350685006028,0.732888284319023,3.50636052923934));
#6856=CARTESIAN_POINT('Ctrl Pts',(1.33775451871254,0.719529169803535,3.48550688646904));
#6857=CARTESIAN_POINT('Ctrl Pts',(1.34215974882296,0.713657162034742,3.47401620307916));
#6858=CARTESIAN_POINT('Ctrl Pts',(1.35490634092634,0.705831016678427,3.45192241458319));
#6859=CARTESIAN_POINT('Ctrl Pts',(1.36324205810433,0.703885991122829,3.44131282688534));
#6860=CARTESIAN_POINT('Ctrl Pts',(1.38100978885234,0.703885991122829,3.42354509613733));
#6861=CARTESIAN_POINT('Ctrl Pts',(1.39161937655019,0.705831016678427,3.41520937895934));
#6862=CARTESIAN_POINT('Ctrl Pts',(1.41371316504616,0.713657162034742,3.40246278685596));
#6863=CARTESIAN_POINT('Ctrl Pts',(1.42520384843604,0.719529169803535,3.39805755674554));
#6864=CARTESIAN_POINT('Ctrl Pts',(1.44605749120634,0.732888284319023,3.39380988809328));
#6865=CARTESIAN_POINT('Ctrl Pts',(1.45681449645766,0.741266387103756,3.39368469084568));
#6866=CARTESIAN_POINT('Ctrl Pts',(1.47592135880746,0.759293157295718,3.39835592477756));
#6867=CARTESIAN_POINT('Ctrl Pts',(1.48427733223337,0.768933614550881,3.40315901402906));
#6868=CARTESIAN_POINT('Ctrl Pts',(1.49055915910216,0.777817459305202,3.40944084089785));
#6869=CARTESIAN_POINT('Ctrl Pts',(1.49055915910215,0.777817459305202,3.40944084089785));
#6870=CARTESIAN_POINT('Ctrl Pts',(1.49684098597094,0.786701304059523,3.41572266776664));
#6871=CARTESIAN_POINT('Ctrl Pts',(1.50188137658261,0.796006166512776,3.4243159425527));
#6872=CARTESIAN_POINT('Ctrl Pts',(1.50741041381927,0.812819819637263,3.44428060820729));
#6873=CARTESIAN_POINT('Ctrl Pts',(1.50789352586237,0.820337643172961,3.45564592274932));
#6874=CARTESIAN_POINT('Ctrl Pts',(1.50478919061565,0.832079840080031,3.47764289892514));
#6875=CARTESIAN_POINT('Ctrl Pts',(1.50099337037799,0.837090012141717,3.48974299218779));
#6876=CARTESIAN_POINT('Ctrl Pts',(1.48910710053031,0.843699478096002,3.51269710293947));
#6877=CARTESIAN_POINT('Ctrl Pts',(1.48100978885234,0.845307347360138,3.52354509613733));
#6878=CARTESIAN_POINT('Ctrl Pts',(1.47212592347833,0.845307347360138,3.53242896151133));
#6879=CARTESIAN_POINT('Origin',(2.00416305603426,-0.848528137423857,5.19583694396574));
#6880=CARTESIAN_POINT('',(2.00188561353943,-0.703885991122829,5.1935595014709));
#6881=CARTESIAN_POINT('',(2.02487373415292,-0.777817459305203,5.07512626584708));
#6882=CARTESIAN_POINT('Ctrl Pts',(2.00188561353943,-0.703885991122828,5.19355950147091));
#6883=CARTESIAN_POINT('Ctrl Pts',(2.01076947891343,-0.703885991122828,5.1846756360969));
#6884=CARTESIAN_POINT('Ctrl Pts',(2.01910519609142,-0.705831016678426,5.17406604839905));
#6885=CARTESIAN_POINT('Ctrl Pts',(2.0318517881948,-0.713657162034741,5.15197225990308));
#6886=CARTESIAN_POINT('Ctrl Pts',(2.03625701830522,-0.719529169803534,5.1404815765132));
#6887=CARTESIAN_POINT('Ctrl Pts',(2.04050468695748,-0.732888284319023,5.1196279337429));
#6888=CARTESIAN_POINT('Ctrl Pts',(2.04062988420509,-0.741266387103756,5.10887092849158));
#6889=CARTESIAN_POINT('Ctrl Pts',(2.0359586502732,-0.759293157295718,5.08976406614178));
#6890=CARTESIAN_POINT('Ctrl Pts',(2.03115556102171,-0.768933614550881,5.08140809271587));
#6891=CARTESIAN_POINT('Ctrl Pts',(2.02487373415292,-0.777817459305202,5.07512626584708));
#6892=CARTESIAN_POINT('Ctrl Pts',(2.02487373415292,-0.777817459305202,5.07512626584708));
#6893=CARTESIAN_POINT('Ctrl Pts',(2.01859190728413,-0.786701304059523,5.0688444389783));
#6894=CARTESIAN_POINT('Ctrl Pts',(2.00999863249806,-0.796006166512776,5.06380404836663));
#6895=CARTESIAN_POINT('Ctrl Pts',(1.99003396684347,-0.812819819637263,5.05827501112997));
#6896=CARTESIAN_POINT('Ctrl Pts',(1.97866865230145,-0.820337643172961,5.05779189908686));
#6897=CARTESIAN_POINT('Ctrl Pts',(1.95667167612562,-0.832079840080031,5.06089623433359));
#6898=CARTESIAN_POINT('Ctrl Pts',(1.94457158286298,-0.837090012141718,5.06469205457125));
#6899=CARTESIAN_POINT('Ctrl Pts',(1.92161747211129,-0.843699478096003,5.07657832441893));
#6900=CARTESIAN_POINT('Ctrl Pts',(1.91076947891343,-0.845307347360138,5.0846756360969));
#6901=CARTESIAN_POINT('Ctrl Pts',(1.89300174816542,-0.845307347360138,5.10244336684491));
#6902=CARTESIAN_POINT('Ctrl Pts',(1.88490443648745,-0.843699478096003,5.11329136004277));
#6903=CARTESIAN_POINT('Ctrl Pts',(1.87301816663977,-0.837090012141718,5.13624547079445));
#6904=CARTESIAN_POINT('Ctrl Pts',(1.86922234640212,-0.832079840080031,5.1483455640571));
#6905=CARTESIAN_POINT('Ctrl Pts',(1.86611801115539,-0.820337643172961,5.17034254023292));
#6906=CARTESIAN_POINT('Ctrl Pts',(1.86660112319849,-0.812819819637263,5.18170785477495));
#6907=CARTESIAN_POINT('Ctrl Pts',(1.87213016043516,-0.796006166512776,5.20167252042954));
#6908=CARTESIAN_POINT('Ctrl Pts',(1.87717055104682,-0.786701304059523,5.21026579521561));
#6909=CARTESIAN_POINT('Ctrl Pts',(1.8897342047844,-0.768933614550882,5.22282944895318));
#6910=CARTESIAN_POINT('Ctrl Pts',(1.8980901782103,-0.759293157295718,5.22763253820468));
#6911=CARTESIAN_POINT('Ctrl Pts',(1.91719704056011,-0.741266387103756,5.23230377213657));
#6912=CARTESIAN_POINT('Ctrl Pts',(1.92795404581142,-0.732888284319023,5.23217857488896));
#6913=CARTESIAN_POINT('Ctrl Pts',(1.94880768858172,-0.719529169803534,5.2279309062367));
#6914=CARTESIAN_POINT('Ctrl Pts',(1.9602983719716,-0.713657162034742,5.22352567612628));
#6915=CARTESIAN_POINT('Ctrl Pts',(1.98239216046757,-0.705831016678426,5.2107790840229));
#6916=CARTESIAN_POINT('Ctrl Pts',(1.99300174816542,-0.703885991122828,5.20244336684491));
#6917=CARTESIAN_POINT('Ctrl Pts',(2.00188561353943,-0.703885991122828,5.19355950147091));
#6918=CARTESIAN_POINT('',(1.97487373415292,-0.707106781186547,5.02512626584708));
#6919=CARTESIAN_POINT('',(2.07487373415292,-0.848528137423857,5.12512626584708));
#6920=CARTESIAN_POINT('',(1.95165677458757,-0.63285168585486,5.14333066251905));
#6921=CARTESIAN_POINT('Ctrl Pts',(1.95165677458757,-0.63285168585486,5.14333066251905));
#6922=CARTESIAN_POINT('Ctrl Pts',(1.94277179351494,-0.632851685854859,5.15221564359168));
#6923=CARTESIAN_POINT('Ctrl Pts',(1.93217349611894,-0.63481421967861,5.16056360077267));
#6924=CARTESIAN_POINT('Ctrl Pts',(1.91012317912779,-0.64270204145114,5.17335304190192));
#6925=CARTESIAN_POINT('Ctrl Pts',(1.89866397622528,-0.648617241117306,5.17778835924145));
#6926=CARTESIAN_POINT('Ctrl Pts',(1.87786971651427,-0.662056333977536,5.18209306664558));
#6927=CARTESIAN_POINT('Ctrl Pts',(1.86714384769216,-0.67047684793714,5.1822490679324));
#6928=CARTESIAN_POINT('Ctrl Pts',(1.84807984227569,-0.688564081560337,5.1776213372919));
#6929=CARTESIAN_POINT('Ctrl Pts',(1.83973498689823,-0.698221830356238,5.17283023106701));
#6930=CARTESIAN_POINT('Ctrl Pts',(1.82716976893299,-0.715991732016857,5.16026501310177));
#6931=CARTESIAN_POINT('Ctrl Pts',(1.8221175838447,-0.725280259543278,5.15165907886091));
#6932=CARTESIAN_POINT('Ctrl Pts',(1.81654611568482,-0.742032846767245,5.13165133592505));
#6933=CARTESIAN_POINT('Ctrl Pts',(1.81603284821736,-0.749506871777696,5.12025619834868));
#6934=CARTESIAN_POINT('Ctrl Pts',(1.81907945808048,-0.76116674603262,5.09820384109664));
#6935=CARTESIAN_POINT('Ctrl Pts',(1.82284404040547,-0.766133383144486,5.0860739031796));
#6936=CARTESIAN_POINT('Ctrl Pts',(1.83468638720153,-0.772681811266156,5.06307649185526));
#6937=CARTESIAN_POINT('Ctrl Pts',(1.84277179351494,-0.774273042092169,5.05221564359168));
#6938=CARTESIAN_POINT('Ctrl Pts',(1.8605417556602,-0.774273042092169,5.03444568144642));
#6939=CARTESIAN_POINT('Ctrl Pts',(1.87140260392378,-0.772681811266156,5.026360275133));
#6940=CARTESIAN_POINT('Ctrl Pts',(1.89440001524813,-0.766133383144486,5.01451792833695));
#6941=CARTESIAN_POINT('Ctrl Pts',(1.90652995316516,-0.761166746032619,5.01075334601195));
#6942=CARTESIAN_POINT('Ctrl Pts',(1.9285823104172,-0.749506871777695,5.00770673614884));
#6943=CARTESIAN_POINT('Ctrl Pts',(1.93997744799358,-0.742032846767245,5.00822000361629));
#6944=CARTESIAN_POINT('Ctrl Pts',(1.95998519092943,-0.725280259543278,5.01379147177617));
#6945=CARTESIAN_POINT('Ctrl Pts',(1.9685911251703,-0.715991732016857,5.01884365686446));
#6946=CARTESIAN_POINT('Ctrl Pts',(1.97487373415292,-0.707106781186548,5.02512626584708));
#6947=CARTESIAN_POINT('Ctrl Pts',(1.97487373415292,-0.707106781186548,5.02512626584708));
#6948=CARTESIAN_POINT('Ctrl Pts',(1.98115634313554,-0.698221830356239,5.0314088748297));
#6949=CARTESIAN_POINT('Ctrl Pts',(1.98594744936042,-0.688564081560337,5.03975373020716));
#6950=CARTESIAN_POINT('Ctrl Pts',(1.99057518000092,-0.67047684793714,5.05881773562364));
#6951=CARTESIAN_POINT('Ctrl Pts',(1.99041917871411,-0.662056333977536,5.06954360444574));
#6952=CARTESIAN_POINT('Ctrl Pts',(1.98611447130997,-0.648617241117307,5.09033786415676));
#6953=CARTESIAN_POINT('Ctrl Pts',(1.98167915397045,-0.642702041451141,5.10179706705927));
#6954=CARTESIAN_POINT('Ctrl Pts',(1.96888971284119,-0.634814219678611,5.12384738405041));
#6955=CARTESIAN_POINT('Ctrl Pts',(1.9605417556602,-0.632851685854859,5.13444568144642));
#6956=CARTESIAN_POINT('Ctrl Pts',(1.95165677458757,-0.632851685854859,5.14333066251905));
#6957=CARTESIAN_POINT('Origin',(2.00416305603426,-0.848528137423857,5.19583694396574));
#6958=CARTESIAN_POINT('',(0.956669337480952,0.774273042092169,4.14834322541243));
#6959=CARTESIAN_POINT('',(0.974873734152917,0.707106781186548,4.02512626584708));
#6960=CARTESIAN_POINT('Ctrl Pts',(0.956669337480952,0.77427304209217,4.14834322541243));
#6961=CARTESIAN_POINT('Ctrl Pts',(0.965554318553584,0.77427304209217,4.1394582443398));
#6962=CARTESIAN_POINT('Ctrl Pts',(0.973639724866999,0.772681811266156,4.12859739607622));
#6963=CARTESIAN_POINT('Ctrl Pts',(0.98548207166305,0.766133383144486,4.10559998475187));
#6964=CARTESIAN_POINT('Ctrl Pts',(0.989246653988049,0.761166746032619,4.09347004683484));
#6965=CARTESIAN_POINT('Ctrl Pts',(0.992293263851161,0.749506871777695,4.0714176895828));
#6966=CARTESIAN_POINT('Ctrl Pts',(0.991779996383709,0.742032846767245,4.06002255200643));
#6967=CARTESIAN_POINT('Ctrl Pts',(0.986208528223828,0.725280259543278,4.04001480907057));
#6968=CARTESIAN_POINT('Ctrl Pts',(0.981156343135538,0.715991732016857,4.0314088748297));
#6969=CARTESIAN_POINT('Ctrl Pts',(0.974873734152917,0.707106781186547,4.02512626584708));
#6970=CARTESIAN_POINT('Ctrl Pts',(0.974873734152917,0.707106781186548,4.02512626584708));
#6971=CARTESIAN_POINT('Ctrl Pts',(0.968591125170296,0.698221830356238,4.01884365686446));
#6972=CARTESIAN_POINT('Ctrl Pts',(0.960246269792838,0.688564081560337,4.01405255063958));
#6973=CARTESIAN_POINT('Ctrl Pts',(0.941182264376365,0.67047684793714,4.00942481999908));
#6974=CARTESIAN_POINT('Ctrl Pts',(0.930456395554258,0.662056333977536,4.00958082128589));
#6975=CARTESIAN_POINT('Ctrl Pts',(0.909662135843242,0.648617241117307,4.01388552869003));
#6976=CARTESIAN_POINT('Ctrl Pts',(0.898202932940732,0.642702041451141,4.01832084602955));
#6977=CARTESIAN_POINT('Ctrl Pts',(0.876152615949588,0.63481421967861,4.03111028715881));
#6978=CARTESIAN_POINT('Ctrl Pts',(0.865554318553583,0.63285168585486,4.0394582443398));
#6979=CARTESIAN_POINT('Ctrl Pts',(0.847784356408321,0.63285168585486,4.05722820648506));
#6980=CARTESIAN_POINT('Ctrl Pts',(0.839436399227331,0.63481421967861,4.06782650388106));
#6981=CARTESIAN_POINT('Ctrl Pts',(0.826646958098078,0.64270204145114,4.08987682087221));
#6982=CARTESIAN_POINT('Ctrl Pts',(0.822211640758555,0.648617241117306,4.10133602377472));
#6983=CARTESIAN_POINT('Ctrl Pts',(0.817906933354418,0.662056333977536,4.12213028348573));
#6984=CARTESIAN_POINT('Ctrl Pts',(0.817750932067606,0.67047684793714,4.13285615230784));
#6985=CARTESIAN_POINT('Ctrl Pts',(0.822378662708104,0.688564081560337,4.15192015772431));
#6986=CARTESIAN_POINT('Ctrl Pts',(0.827169768932986,0.698221830356238,4.16026501310177));
#6987=CARTESIAN_POINT('Ctrl Pts',(0.839734986898228,0.715991732016857,4.17283023106701));
#6988=CARTESIAN_POINT('Ctrl Pts',(0.848340921139093,0.725280259543278,4.1778824161553));
#6989=CARTESIAN_POINT('Ctrl Pts',(0.86834866407495,0.742032846767245,4.18345388431518));
#6990=CARTESIAN_POINT('Ctrl Pts',(0.879743801651321,0.749506871777696,4.18396715178264));
#6991=CARTESIAN_POINT('Ctrl Pts',(0.901796158903362,0.76116674603262,4.18092054191952));
#6992=CARTESIAN_POINT('Ctrl Pts',(0.913926096820397,0.766133383144486,4.17715595959453));
#6993=CARTESIAN_POINT('Ctrl Pts',(0.936923508144742,0.772681811266156,4.16531361279847));
#6994=CARTESIAN_POINT('Ctrl Pts',(0.947784356408321,0.774273042092169,4.15722820648506));
#6995=CARTESIAN_POINT('Ctrl Pts',(0.956669337480952,0.774273042092169,4.14834322541243));
#6996=CARTESIAN_POINT('',(0.924873734152917,0.777817459305203,3.97512626584708));
#6997=CARTESIAN_POINT('',(2.07487373415292,-0.848528137423857,5.12512626584708));
#6998=CARTESIAN_POINT('',(0.906440498529096,0.845307347360138,4.09811438646057));
#6999=CARTESIAN_POINT('Ctrl Pts',(0.906440498529096,0.845307347360138,4.09811438646057));
#7000=CARTESIAN_POINT('Ctrl Pts',(0.89755663315509,0.845307347360138,4.10699825183458));
#7001=CARTESIAN_POINT('Ctrl Pts',(0.886708639957229,0.843699478096003,4.11509556351255));
#7002=CARTESIAN_POINT('Ctrl Pts',(0.863754529205548,0.837090012141718,4.12698183336023));
#7003=CARTESIAN_POINT('Ctrl Pts',(0.851654435942905,0.832079840080031,4.13077765359789));
#7004=CARTESIAN_POINT('Ctrl Pts',(0.829657459767076,0.820337643172961,4.13388198884461));
#7005=CARTESIAN_POINT('Ctrl Pts',(0.818292145225052,0.812819819637263,4.13339887680151));
#7006=CARTESIAN_POINT('Ctrl Pts',(0.798327479570465,0.796006166512776,4.12786983956484));
#7007=CARTESIAN_POINT('Ctrl Pts',(0.789734204784396,0.786701304059523,4.12282944895318));
#7008=CARTESIAN_POINT('Ctrl Pts',(0.777170551046818,0.768933614550881,4.1102657952156));
#7009=CARTESIAN_POINT('Ctrl Pts',(0.77236746179532,0.759293157295718,4.1019098217897));
#7010=CARTESIAN_POINT('Ctrl Pts',(0.767696227863436,0.741266387103756,4.08280295943989));
#7011=CARTESIAN_POINT('Ctrl Pts',(0.76782142511104,0.732888284319023,4.07204595418858));
#7012=CARTESIAN_POINT('Ctrl Pts',(0.772069093763303,0.719529169803534,4.05119231141828));
#7013=CARTESIAN_POINT('Ctrl Pts',(0.776474323873723,0.713657162034741,4.0397016280284));
#7014=CARTESIAN_POINT('Ctrl Pts',(0.789220915977106,0.705831016678426,4.01760783953243));
#7015=CARTESIAN_POINT('Ctrl Pts',(0.797556633155091,0.703885991122829,4.00699825183458));
#7016=CARTESIAN_POINT('Ctrl Pts',(0.815324363903101,0.703885991122829,3.98923052108657));
#7017=CARTESIAN_POINT('Ctrl Pts',(0.82593395160095,0.705831016678427,3.98089480390858));
#7018=CARTESIAN_POINT('Ctrl Pts',(0.848027740096926,0.713657162034742,3.9681482118052));
#7019=CARTESIAN_POINT('Ctrl Pts',(0.859518423486806,0.719529169803534,3.96374298169478));
#7020=CARTESIAN_POINT('Ctrl Pts',(0.880372066257101,0.732888284319023,3.95949531304252));
#7021=CARTESIAN_POINT('Ctrl Pts',(0.891129071508419,0.741266387103756,3.95937011579491));
#7022=CARTESIAN_POINT('Ctrl Pts',(0.910235933858221,0.759293157295718,3.9640413497268));
#7023=CARTESIAN_POINT('Ctrl Pts',(0.918591907284128,0.768933614550881,3.96884443897829));
#7024=CARTESIAN_POINT('Ctrl Pts',(0.924873734152917,0.777817459305202,3.97512626584708));
#7025=CARTESIAN_POINT('Ctrl Pts',(0.924873734152917,0.777817459305202,3.97512626584708));
#7026=CARTESIAN_POINT('Ctrl Pts',(0.931155561021706,0.786701304059523,3.98140809271587));
#7027=CARTESIAN_POINT('Ctrl Pts',(0.936195951633367,0.796006166512776,3.99000136750194));
#7028=CARTESIAN_POINT('Ctrl Pts',(0.941724988870036,0.812819819637263,4.00996603315653));
#7029=CARTESIAN_POINT('Ctrl Pts',(0.942208100913137,0.820337643172961,4.02133134769855));
#7030=CARTESIAN_POINT('Ctrl Pts',(0.939103765666408,0.832079840080031,4.04332832387438));
#7031=CARTESIAN_POINT('Ctrl Pts',(0.935307945428751,0.837090012141718,4.05542841713703));
#7032=CARTESIAN_POINT('Ctrl Pts',(0.923421675581074,0.843699478096003,4.07838252788871));
#7033=CARTESIAN_POINT('Ctrl Pts',(0.915324363903102,0.845307347360138,4.08923052108657));
#7034=CARTESIAN_POINT('Ctrl Pts',(0.906440498529096,0.845307347360138,4.09811438646057));
#7035=CARTESIAN_POINT('Origin',(1.43847763108502,-0.848528137423857,5.76152236891498));
#7036=CARTESIAN_POINT('',(1.43620018859019,-0.703885991122829,5.75924492642014));
#7037=CARTESIAN_POINT('',(1.45918830920368,-0.777817459305203,5.64081169079632));
#7038=CARTESIAN_POINT('Ctrl Pts',(1.43620018859019,-0.703885991122829,5.75924492642014));
#7039=CARTESIAN_POINT('Ctrl Pts',(1.4450840539642,-0.703885991122829,5.75036106104614));
#7040=CARTESIAN_POINT('Ctrl Pts',(1.45341977114218,-0.705831016678426,5.73975147334829));
#7041=CARTESIAN_POINT('Ctrl Pts',(1.46616636324556,-0.713657162034741,5.71765768485231));
#7042=CARTESIAN_POINT('Ctrl Pts',(1.47057159335598,-0.719529169803534,5.70616700146243));
#7043=CARTESIAN_POINT('Ctrl Pts',(1.47481926200825,-0.732888284319023,5.68531335869214));
#7044=CARTESIAN_POINT('Ctrl Pts',(1.47494445925585,-0.741266387103756,5.67455635344082));
#7045=CARTESIAN_POINT('Ctrl Pts',(1.47027322532397,-0.759293157295718,5.65544949109102));
#7046=CARTESIAN_POINT('Ctrl Pts',(1.46547013607247,-0.768933614550882,5.64709351766511));
#7047=CARTESIAN_POINT('Ctrl Pts',(1.45918830920368,-0.777817459305203,5.64081169079632));
#7048=CARTESIAN_POINT('Ctrl Pts',(1.45918830920368,-0.777817459305203,5.64081169079632));
#7049=CARTESIAN_POINT('Ctrl Pts',(1.45290648233489,-0.786701304059524,5.63452986392753));
#7050=CARTESIAN_POINT('Ctrl Pts',(1.44431320754882,-0.796006166512776,5.62948947331587));
#7051=CARTESIAN_POINT('Ctrl Pts',(1.42434854189423,-0.812819819637263,5.6239604360792));
#7052=CARTESIAN_POINT('Ctrl Pts',(1.41298322735221,-0.820337643172961,5.6234773240361));
#7053=CARTESIAN_POINT('Ctrl Pts',(1.39098625117638,-0.832079840080031,5.62658165928283));
#7054=CARTESIAN_POINT('Ctrl Pts',(1.37888615791374,-0.837090012141717,5.63037747952049));
#7055=CARTESIAN_POINT('Ctrl Pts',(1.35593204716206,-0.843699478096003,5.64226374936816));
#7056=CARTESIAN_POINT('Ctrl Pts',(1.3450840539642,-0.845307347360138,5.65036106104614));
#7057=CARTESIAN_POINT('Ctrl Pts',(1.32731632321618,-0.845307347360138,5.66812879179415));
#7058=CARTESIAN_POINT('Ctrl Pts',(1.31921901153821,-0.843699478096003,5.67897678499201));
#7059=CARTESIAN_POINT('Ctrl Pts',(1.30733274169054,-0.837090012141718,5.70193089574369));
#7060=CARTESIAN_POINT('Ctrl Pts',(1.30353692145288,-0.832079840080031,5.71403098900633));
#7061=CARTESIAN_POINT('Ctrl Pts',(1.30043258620615,-0.820337643172961,5.73602796518216));
#7062=CARTESIAN_POINT('Ctrl Pts',(1.30091569824925,-0.812819819637263,5.74739327972419));
#7063=CARTESIAN_POINT('Ctrl Pts',(1.30644473548592,-0.796006166512776,5.76735794537877));
#7064=CARTESIAN_POINT('Ctrl Pts',(1.31148512609758,-0.786701304059523,5.77595122016484));
#7065=CARTESIAN_POINT('Ctrl Pts',(1.32404877983516,-0.768933614550882,5.78851487390242));
#7066=CARTESIAN_POINT('Ctrl Pts',(1.33240475326106,-0.759293157295718,5.79331796315392));
#7067=CARTESIAN_POINT('Ctrl Pts',(1.35151161561087,-0.741266387103756,5.7979891970858));
#7068=CARTESIAN_POINT('Ctrl Pts',(1.36226862086218,-0.732888284319023,5.7978639998382));
#7069=CARTESIAN_POINT('Ctrl Pts',(1.38312226363248,-0.719529169803534,5.79361633118594));
#7070=CARTESIAN_POINT('Ctrl Pts',(1.39461294702236,-0.713657162034741,5.78921110107552));
#7071=CARTESIAN_POINT('Ctrl Pts',(1.41670673551834,-0.705831016678426,5.77646450897213));
#7072=CARTESIAN_POINT('Ctrl Pts',(1.42731632321618,-0.703885991122829,5.76812879179415));
#7073=CARTESIAN_POINT('Ctrl Pts',(1.43620018859019,-0.703885991122829,5.75924492642014));
#7074=CARTESIAN_POINT('',(1.40918830920368,-0.707106781186548,5.59081169079632));
#7075=CARTESIAN_POINT('',(1.50918830920368,-0.848528137423857,5.69081169079632));
#7076=CARTESIAN_POINT('',(1.38597134963833,-0.63285168585486,5.70901608746829));
#7077=CARTESIAN_POINT('Ctrl Pts',(1.38597134963833,-0.63285168585486,5.70901608746829));
#7078=CARTESIAN_POINT('Ctrl Pts',(1.3770863685657,-0.63285168585486,5.71790106854092));
#7079=CARTESIAN_POINT('Ctrl Pts',(1.3664880711697,-0.634814219678611,5.72624902572191));
#7080=CARTESIAN_POINT('Ctrl Pts',(1.34443775417856,-0.642702041451141,5.73903846685116));
#7081=CARTESIAN_POINT('Ctrl Pts',(1.33297855127604,-0.648617241117306,5.74347378419068));
#7082=CARTESIAN_POINT('Ctrl Pts',(1.31218429156503,-0.662056333977536,5.74777849159482));
#7083=CARTESIAN_POINT('Ctrl Pts',(1.30145842274292,-0.67047684793714,5.74793449288163));
#7084=CARTESIAN_POINT('Ctrl Pts',(1.28239441732645,-0.688564081560337,5.74330676224113));
#7085=CARTESIAN_POINT('Ctrl Pts',(1.27404956194899,-0.698221830356238,5.73851565601625));
#7086=CARTESIAN_POINT('Ctrl Pts',(1.26148434398375,-0.715991732016857,5.72595043805101));
#7087=CARTESIAN_POINT('Ctrl Pts',(1.25643215889546,-0.725280259543277,5.71734450381014));
#7088=CARTESIAN_POINT('Ctrl Pts',(1.25086069073558,-0.742032846767245,5.69733676087429));
#7089=CARTESIAN_POINT('Ctrl Pts',(1.25034742326813,-0.749506871777696,5.68594162329792));
#7090=CARTESIAN_POINT('Ctrl Pts',(1.25339403313124,-0.76116674603262,5.66388926604588));
#7091=CARTESIAN_POINT('Ctrl Pts',(1.25715861545624,-0.766133383144486,5.65175932812884));
#7092=CARTESIAN_POINT('Ctrl Pts',(1.26900096225229,-0.772681811266156,5.6287619168045));
#7093=CARTESIAN_POINT('Ctrl Pts',(1.2770863685657,-0.774273042092169,5.61790106854092));
#7094=CARTESIAN_POINT('Ctrl Pts',(1.29485633071097,-0.774273042092169,5.60013110639566));
#7095=CARTESIAN_POINT('Ctrl Pts',(1.30571717897454,-0.772681811266156,5.59204570008224));
#7096=CARTESIAN_POINT('Ctrl Pts',(1.32871459029889,-0.766133383144486,5.58020335328619));
#7097=CARTESIAN_POINT('Ctrl Pts',(1.34084452821592,-0.76116674603262,5.57643877096119));
#7098=CARTESIAN_POINT('Ctrl Pts',(1.36289688546797,-0.749506871777696,5.57339216109808));
#7099=CARTESIAN_POINT('Ctrl Pts',(1.37429202304434,-0.742032846767245,5.57390542856553));
#7100=CARTESIAN_POINT('Ctrl Pts',(1.39429976598019,-0.725280259543277,5.57947689672541));
#7101=CARTESIAN_POINT('Ctrl Pts',(1.40290570022106,-0.715991732016857,5.5845290818137));
#7102=CARTESIAN_POINT('Ctrl Pts',(1.40918830920368,-0.707106781186548,5.59081169079632));
#7103=CARTESIAN_POINT('Ctrl Pts',(1.40918830920368,-0.707106781186548,5.59081169079632));
#7104=CARTESIAN_POINT('Ctrl Pts',(1.4154709181863,-0.698221830356238,5.59709429977894));
#7105=CARTESIAN_POINT('Ctrl Pts',(1.42026202441118,-0.688564081560337,5.6054391551564));
#7106=CARTESIAN_POINT('Ctrl Pts',(1.42488975505168,-0.67047684793714,5.62450316057287));
#7107=CARTESIAN_POINT('Ctrl Pts',(1.42473375376487,-0.662056333977536,5.63522902939498));
#7108=CARTESIAN_POINT('Ctrl Pts',(1.42042904636073,-0.648617241117306,5.656023289106));
#7109=CARTESIAN_POINT('Ctrl Pts',(1.41599372902121,-0.642702041451141,5.66748249200851));
#7110=CARTESIAN_POINT('Ctrl Pts',(1.40320428789196,-0.634814219678611,5.68953280899965));
#7111=CARTESIAN_POINT('Ctrl Pts',(1.39485633071096,-0.63285168585486,5.70013110639566));
#7112=CARTESIAN_POINT('Ctrl Pts',(1.38597134963833,-0.63285168585486,5.70901608746829));
#7113=CARTESIAN_POINT('Origin',(1.43847763108502,-0.848528137423857,5.76152236891498));
#7114=CARTESIAN_POINT('',(0.390983912531714,0.774273042092169,4.71402865036167));
#7115=CARTESIAN_POINT('',(0.409188309203679,0.707106781186548,4.59081169079632));
#7116=CARTESIAN_POINT('Ctrl Pts',(0.390983912531714,0.774273042092169,4.71402865036167));
#7117=CARTESIAN_POINT('Ctrl Pts',(0.399868893604345,0.774273042092169,4.70514366928904));
#7118=CARTESIAN_POINT('Ctrl Pts',(0.407954299917761,0.772681811266156,4.69428282102546));
#7119=CARTESIAN_POINT('Ctrl Pts',(0.419796646713812,0.766133383144486,4.67128540970111));
#7120=CARTESIAN_POINT('Ctrl Pts',(0.42356122903881,0.76116674603262,4.65915547178408));
#7121=CARTESIAN_POINT('Ctrl Pts',(0.426607838901923,0.749506871777696,4.63710311453204));
#7122=CARTESIAN_POINT('Ctrl Pts',(0.426094571434471,0.742032846767245,4.62570797695566));
#7123=CARTESIAN_POINT('Ctrl Pts',(0.42052310327459,0.725280259543278,4.60570023401981));
#7124=CARTESIAN_POINT('Ctrl Pts',(0.4154709181863,0.715991732016857,4.59709429977894));
#7125=CARTESIAN_POINT('Ctrl Pts',(0.409188309203679,0.707106781186548,4.59081169079632));
#7126=CARTESIAN_POINT('Ctrl Pts',(0.409188309203679,0.707106781186548,4.59081169079632));
#7127=CARTESIAN_POINT('Ctrl Pts',(0.402905700221058,0.698221830356238,4.5845290818137));
#7128=CARTESIAN_POINT('Ctrl Pts',(0.394560844843601,0.688564081560337,4.57973797558882));
#7129=CARTESIAN_POINT('Ctrl Pts',(0.375496839427127,0.67047684793714,4.57511024494832));
#7130=CARTESIAN_POINT('Ctrl Pts',(0.36477097060502,0.662056333977536,4.57526624623513));
#7131=CARTESIAN_POINT('Ctrl Pts',(0.343976710894004,0.648617241117306,4.57957095363927));
#7132=CARTESIAN_POINT('Ctrl Pts',(0.332517507991493,0.642702041451141,4.58400627097879));
#7133=CARTESIAN_POINT('Ctrl Pts',(0.310467191000349,0.63481421967861,4.59679571210804));
#7134=CARTESIAN_POINT('Ctrl Pts',(0.299868893604345,0.63285168585486,4.60514366928903));
#7135=CARTESIAN_POINT('Ctrl Pts',(0.282098931459083,0.63285168585486,4.6229136314343));
#7136=CARTESIAN_POINT('Ctrl Pts',(0.273750974278093,0.63481421967861,4.6335119288303));
#7137=CARTESIAN_POINT('Ctrl Pts',(0.26096153314884,0.642702041451141,4.65556224582144));
#7138=CARTESIAN_POINT('Ctrl Pts',(0.256526215809317,0.648617241117306,4.66702144872396));
#7139=CARTESIAN_POINT('Ctrl Pts',(0.252221508405179,0.662056333977536,4.68781570843497));
#7140=CARTESIAN_POINT('Ctrl Pts',(0.252065507118367,0.67047684793714,4.69854157725708));
#7141=CARTESIAN_POINT('Ctrl Pts',(0.256693237758866,0.688564081560337,4.71760558267355));
#7142=CARTESIAN_POINT('Ctrl Pts',(0.261484343983749,0.698221830356238,4.72595043805101));
#7143=CARTESIAN_POINT('Ctrl Pts',(0.27404956194899,0.715991732016857,4.73851565601625));
#7144=CARTESIAN_POINT('Ctrl Pts',(0.282655496189856,0.725280259543277,4.74356784110454));
#7145=CARTESIAN_POINT('Ctrl Pts',(0.302663239125711,0.742032846767245,4.74913930926442));
#7146=CARTESIAN_POINT('Ctrl Pts',(0.314058376702083,0.749506871777696,4.74965257673188));
#7147=CARTESIAN_POINT('Ctrl Pts',(0.336110733954123,0.76116674603262,4.74660596686876));
#7148=CARTESIAN_POINT('Ctrl Pts',(0.348240671871159,0.766133383144486,4.74284138454376));
#7149=CARTESIAN_POINT('Ctrl Pts',(0.371238083195504,0.772681811266156,4.73099903774771));
#7150=CARTESIAN_POINT('Ctrl Pts',(0.382098931459083,0.774273042092169,4.7229136314343));
#7151=CARTESIAN_POINT('Ctrl Pts',(0.390983912531714,0.774273042092169,4.71402865036167));
#7152=CARTESIAN_POINT('',(0.359188309203679,0.777817459305203,4.54081169079632));
#7153=CARTESIAN_POINT('',(1.50918830920368,-0.848528137423857,5.69081169079632));
#7154=CARTESIAN_POINT('',(0.340755073579858,0.845307347360138,4.66379981140981));
#7155=CARTESIAN_POINT('Ctrl Pts',(0.340755073579858,0.845307347360138,4.66379981140981));
#7156=CARTESIAN_POINT('Ctrl Pts',(0.331871208205852,0.845307347360138,4.67268367678381));
#7157=CARTESIAN_POINT('Ctrl Pts',(0.321023215007992,0.843699478096003,4.68078098846179));
#7158=CARTESIAN_POINT('Ctrl Pts',(0.29806910425631,0.837090012141718,4.69266725830947));
#7159=CARTESIAN_POINT('Ctrl Pts',(0.285969010993667,0.832079840080031,4.69646307854712));
#7160=CARTESIAN_POINT('Ctrl Pts',(0.263972034817838,0.820337643172961,4.69956741379385));
#7161=CARTESIAN_POINT('Ctrl Pts',(0.252606720275814,0.812819819637263,4.69908430175075));
#7162=CARTESIAN_POINT('Ctrl Pts',(0.232642054621227,0.796006166512776,4.69355526451408));
#7163=CARTESIAN_POINT('Ctrl Pts',(0.224048779835158,0.786701304059523,4.68851487390242));
#7164=CARTESIAN_POINT('Ctrl Pts',(0.211485126097581,0.768933614550881,4.67595122016484));
#7165=CARTESIAN_POINT('Ctrl Pts',(0.206682036846082,0.759293157295718,4.66759524673894));
#7166=CARTESIAN_POINT('Ctrl Pts',(0.202010802914198,0.741266387103756,4.64848838438913));
#7167=CARTESIAN_POINT('Ctrl Pts',(0.202136000161802,0.732888284319023,4.63773137913782));
#7168=CARTESIAN_POINT('Ctrl Pts',(0.206383668814065,0.719529169803534,4.61687773636752));
#7169=CARTESIAN_POINT('Ctrl Pts',(0.210788898924485,0.713657162034741,4.60538705297764));
#7170=CARTESIAN_POINT('Ctrl Pts',(0.223535491027868,0.705831016678426,4.58329326448166));
#7171=CARTESIAN_POINT('Ctrl Pts',(0.231871208205852,0.703885991122829,4.57268367678382));
#7172=CARTESIAN_POINT('Ctrl Pts',(0.249638938953864,0.703885991122829,4.5549159460358));
#7173=CARTESIAN_POINT('Ctrl Pts',(0.260248526651712,0.705831016678426,4.54658022885782));
#7174=CARTESIAN_POINT('Ctrl Pts',(0.282342315147688,0.713657162034741,4.53383363675444));
#7175=CARTESIAN_POINT('Ctrl Pts',(0.293832998537568,0.719529169803534,4.52942840664402));
#7176=CARTESIAN_POINT('Ctrl Pts',(0.314686641307864,0.732888284319023,4.52518073799175));
#7177=CARTESIAN_POINT('Ctrl Pts',(0.325443646559181,0.741266387103756,4.52505554074415));
#7178=CARTESIAN_POINT('Ctrl Pts',(0.344550508908983,0.759293157295718,4.52972677467603));
#7179=CARTESIAN_POINT('Ctrl Pts',(0.352906482334891,0.768933614550882,4.53452986392753));
#7180=CARTESIAN_POINT('Ctrl Pts',(0.359188309203679,0.777817459305202,4.54081169079632));
#7181=CARTESIAN_POINT('Ctrl Pts',(0.359188309203679,0.777817459305202,4.54081169079632));
#7182=CARTESIAN_POINT('Ctrl Pts',(0.365470136072468,0.786701304059523,4.54709351766511));
#7183=CARTESIAN_POINT('Ctrl Pts',(0.37051052668413,0.796006166512776,4.55568679245118));
#7184=CARTESIAN_POINT('Ctrl Pts',(0.376039563920798,0.812819819637263,4.57565145810577));
#7185=CARTESIAN_POINT('Ctrl Pts',(0.3765226759639,0.820337643172961,4.58701677264779));
#7186=CARTESIAN_POINT('Ctrl Pts',(0.37341834071717,0.832079840080031,4.60901374882362));
#7187=CARTESIAN_POINT('Ctrl Pts',(0.369622520479513,0.837090012141718,4.62111384208626));
#7188=CARTESIAN_POINT('Ctrl Pts',(0.357736250631836,0.843699478096003,4.64406795283794));
#7189=CARTESIAN_POINT('Ctrl Pts',(0.349638938953863,0.845307347360138,4.6549159460358));
#7190=CARTESIAN_POINT('Ctrl Pts',(0.340755073579858,0.845307347360138,4.66379981140981));
#7191=CARTESIAN_POINT('Origin',(0.872792206135786,-0.848528137423857,6.32720779386421));
#7192=CARTESIAN_POINT('',(0.870514763640952,-0.703885991122829,6.32493035136938));
#7193=CARTESIAN_POINT('',(0.893502884254441,-0.777817459305203,6.20649711574556));
#7194=CARTESIAN_POINT('Ctrl Pts',(0.870514763640952,-0.703885991122829,
6.32493035136938));
#7195=CARTESIAN_POINT('Ctrl Pts',(0.879398629014957,-0.703885991122829,
6.31604648599538));
#7196=CARTESIAN_POINT('Ctrl Pts',(0.887734346192942,-0.705831016678426,
6.30543689829753));
#7197=CARTESIAN_POINT('Ctrl Pts',(0.900480938296325,-0.713657162034742,
6.28334310980155));
#7198=CARTESIAN_POINT('Ctrl Pts',(0.904886168406745,-0.719529169803534,
6.27185242641167));
#7199=CARTESIAN_POINT('Ctrl Pts',(0.909133837059008,-0.732888284319023,
6.25099878364137));
#7200=CARTESIAN_POINT('Ctrl Pts',(0.909259034306612,-0.741266387103756,
6.24024177839006));
#7201=CARTESIAN_POINT('Ctrl Pts',(0.904587800374729,-0.759293157295718,
6.22113491604026));
#7202=CARTESIAN_POINT('Ctrl Pts',(0.899784711123229,-0.768933614550882,
6.21277894261435));
#7203=CARTESIAN_POINT('Ctrl Pts',(0.89350288425444,-0.777817459305203,6.20649711574556));
#7204=CARTESIAN_POINT('Ctrl Pts',(0.893502884254441,-0.777817459305203,
6.20649711574556));
#7205=CARTESIAN_POINT('Ctrl Pts',(0.887221057385652,-0.786701304059523,
6.20021528887677));
#7206=CARTESIAN_POINT('Ctrl Pts',(0.878627782599582,-0.796006166512776,
6.19517489826511));
#7207=CARTESIAN_POINT('Ctrl Pts',(0.858663116944995,-0.812819819637263,
6.18964586102844));
#7208=CARTESIAN_POINT('Ctrl Pts',(0.847297802402972,-0.820337643172961,
6.18916274898534));
#7209=CARTESIAN_POINT('Ctrl Pts',(0.825300826227143,-0.832079840080031,
6.19226708423207));
#7210=CARTESIAN_POINT('Ctrl Pts',(0.8132007329645,-0.837090012141717,6.19606290446973));
#7211=CARTESIAN_POINT('Ctrl Pts',(0.790246622212818,-0.843699478096003,
6.2079491743174));
#7212=CARTESIAN_POINT('Ctrl Pts',(0.779398629014957,-0.845307347360138,
6.21604648599538));
#7213=CARTESIAN_POINT('Ctrl Pts',(0.761630898266946,-0.845307347360138,
6.23381421674339));
#7214=CARTESIAN_POINT('Ctrl Pts',(0.753533586588974,-0.843699478096003,
6.24466220994125));
#7215=CARTESIAN_POINT('Ctrl Pts',(0.741647316741297,-0.837090012141718,
6.26761632069293));
#7216=CARTESIAN_POINT('Ctrl Pts',(0.73785149650364,-0.832079840080031,6.27971641395557));
#7217=CARTESIAN_POINT('Ctrl Pts',(0.73474716125691,-0.820337643172961,6.3017133901314));
#7218=CARTESIAN_POINT('Ctrl Pts',(0.735230273300012,-0.812819819637263,
6.31307870467342));
#7219=CARTESIAN_POINT('Ctrl Pts',(0.740759310536681,-0.796006166512776,
6.33304337032801));
#7220=CARTESIAN_POINT('Ctrl Pts',(0.745799701148342,-0.786701304059523,
6.34163664511408));
#7221=CARTESIAN_POINT('Ctrl Pts',(0.75836335488592,-0.768933614550882,6.35420029885166));
#7222=CARTESIAN_POINT('Ctrl Pts',(0.766719328311827,-0.759293157295718,
6.35900338810316));
#7223=CARTESIAN_POINT('Ctrl Pts',(0.785826190661629,-0.741266387103756,
6.36367462203504));
#7224=CARTESIAN_POINT('Ctrl Pts',(0.796583195912946,-0.732888284319023,
6.36354942478744));
#7225=CARTESIAN_POINT('Ctrl Pts',(0.817436838683242,-0.719529169803534,
6.35930175613517));
#7226=CARTESIAN_POINT('Ctrl Pts',(0.828927522073122,-0.713657162034742,
6.35489652602475));
#7227=CARTESIAN_POINT('Ctrl Pts',(0.851021310569098,-0.705831016678426,
6.34214993392137));
#7228=CARTESIAN_POINT('Ctrl Pts',(0.861630898266946,-0.703885991122829,
6.33381421674339));
#7229=CARTESIAN_POINT('Ctrl Pts',(0.870514763640952,-0.703885991122829,
6.32493035136938));
#7230=CARTESIAN_POINT('',(0.84350288425444,-0.707106781186548,6.15649711574556));
#7231=CARTESIAN_POINT('',(0.943502884254441,-0.848528137423857,6.25649711574556));
#7232=CARTESIAN_POINT('',(0.820285924689096,-0.63285168585486,6.27470151241752));
#7233=CARTESIAN_POINT('Ctrl Pts',(0.820285924689096,-0.63285168585486,6.27470151241753));
#7234=CARTESIAN_POINT('Ctrl Pts',(0.811400943616464,-0.63285168585486,6.28358649349016));
#7235=CARTESIAN_POINT('Ctrl Pts',(0.80080264622046,-0.634814219678611,6.29193445067115));
#7236=CARTESIAN_POINT('Ctrl Pts',(0.778752329229317,-0.642702041451141,
6.3047238918004));
#7237=CARTESIAN_POINT('Ctrl Pts',(0.767293126326806,-0.648617241117306,
6.30915920913992));
#7238=CARTESIAN_POINT('Ctrl Pts',(0.74649886661579,-0.662056333977536,6.31346391654406));
#7239=CARTESIAN_POINT('Ctrl Pts',(0.735772997793683,-0.67047684793714,6.31361991783087));
#7240=CARTESIAN_POINT('Ctrl Pts',(0.716708992377209,-0.688564081560337,
6.30899218719037));
#7241=CARTESIAN_POINT('Ctrl Pts',(0.708364136999752,-0.698221830356238,
6.30420108096549));
#7242=CARTESIAN_POINT('Ctrl Pts',(0.69579891903451,-0.715991732016857,6.29163586300025));
#7243=CARTESIAN_POINT('Ctrl Pts',(0.69074673394622,-0.725280259543277,6.28302992875938));
#7244=CARTESIAN_POINT('Ctrl Pts',(0.685175265786339,-0.742032846767245,
6.26302218582353));
#7245=CARTESIAN_POINT('Ctrl Pts',(0.684661998318887,-0.749506871777696,
6.25162704824716));
#7246=CARTESIAN_POINT('Ctrl Pts',(0.687708608181999,-0.76116674603262,6.22957469099512));
#7247=CARTESIAN_POINT('Ctrl Pts',(0.691473190506998,-0.766133383144486,
6.21744475307808));
#7248=CARTESIAN_POINT('Ctrl Pts',(0.70331553730305,-0.772681811266156,6.19444734175373));
#7249=CARTESIAN_POINT('Ctrl Pts',(0.711400943616465,-0.774273042092169,
6.18358649349016));
#7250=CARTESIAN_POINT('Ctrl Pts',(0.729170905761727,-0.774273042092169,
6.16581653134489));
#7251=CARTESIAN_POINT('Ctrl Pts',(0.740031754025307,-0.772681811266156,
6.15773112503148));
#7252=CARTESIAN_POINT('Ctrl Pts',(0.763029165349651,-0.766133383144486,
6.14588877823543));
#7253=CARTESIAN_POINT('Ctrl Pts',(0.775159103266687,-0.76116674603262,6.14212419591043));
#7254=CARTESIAN_POINT('Ctrl Pts',(0.797211460518727,-0.749506871777696,
6.13907758604732));
#7255=CARTESIAN_POINT('Ctrl Pts',(0.808606598095099,-0.742032846767245,
6.13959085351477));
#7256=CARTESIAN_POINT('Ctrl Pts',(0.828614341030955,-0.725280259543277,
6.14516232167465));
#7257=CARTESIAN_POINT('Ctrl Pts',(0.83722027527182,-0.715991732016857,6.15021450676294));
#7258=CARTESIAN_POINT('Ctrl Pts',(0.843502884254441,-0.707106781186547,
6.15649711574556));
#7259=CARTESIAN_POINT('Ctrl Pts',(0.843502884254441,-0.707106781186548,
6.15649711574556));
#7260=CARTESIAN_POINT('Ctrl Pts',(0.849785493237061,-0.698221830356239,
6.16277972472818));
#7261=CARTESIAN_POINT('Ctrl Pts',(0.854576599461943,-0.688564081560337,
6.17112458010564));
#7262=CARTESIAN_POINT('Ctrl Pts',(0.859204330102443,-0.67047684793714,6.19018858552211));
#7263=CARTESIAN_POINT('Ctrl Pts',(0.859048328815631,-0.662056333977536,
6.20091445434422));
#7264=CARTESIAN_POINT('Ctrl Pts',(0.854743621411493,-0.648617241117306,
6.22170871405523));
#7265=CARTESIAN_POINT('Ctrl Pts',(0.85030830407197,-0.642702041451141,6.23316791695775));
#7266=CARTESIAN_POINT('Ctrl Pts',(0.837518862942717,-0.63481421967861,6.25521823394889));
#7267=CARTESIAN_POINT('Ctrl Pts',(0.829170905761727,-0.63285168585486,6.26581653134489));
#7268=CARTESIAN_POINT('Ctrl Pts',(0.820285924689096,-0.63285168585486,6.27470151241752));
#7269=CARTESIAN_POINT('Origin',(0.872792206135786,-0.848528137423857,6.32720779386421));
#7270=CARTESIAN_POINT('',(-0.174701512417524,0.774273042092169,5.2797140753109));
#7271=CARTESIAN_POINT('',(-0.156497115745559,0.707106781186548,5.15649711574556));
#7272=CARTESIAN_POINT('Ctrl Pts',(-0.174701512417524,0.774273042092169,
5.2797140753109));
#7273=CARTESIAN_POINT('Ctrl Pts',(-0.165816531344893,0.774273042092169,
5.27082909423827));
#7274=CARTESIAN_POINT('Ctrl Pts',(-0.157731125031478,0.772681811266156,
5.25996824597469));
#7275=CARTESIAN_POINT('Ctrl Pts',(-0.145888778235427,0.766133383144486,
5.23697083465035));
#7276=CARTESIAN_POINT('Ctrl Pts',(-0.142124195910428,0.76116674603262,5.22484089673331));
#7277=CARTESIAN_POINT('Ctrl Pts',(-0.139077586047315,0.749506871777696,
5.20278853948127));
#7278=CARTESIAN_POINT('Ctrl Pts',(-0.139590853514767,0.742032846767245,
5.1913934019049));
#7279=CARTESIAN_POINT('Ctrl Pts',(-0.145162321674648,0.725280259543277,
5.17138565896905));
#7280=CARTESIAN_POINT('Ctrl Pts',(-0.150214506762938,0.715991732016857,
5.16277972472818));
#7281=CARTESIAN_POINT('Ctrl Pts',(-0.156497115745559,0.707106781186548,
5.15649711574556));
#7282=CARTESIAN_POINT('Ctrl Pts',(-0.156497115745559,0.707106781186548,
5.15649711574556));
#7283=CARTESIAN_POINT('Ctrl Pts',(-0.16277972472818,0.698221830356239,5.15021450676294));
#7284=CARTESIAN_POINT('Ctrl Pts',(-0.171124580105637,0.688564081560337,
5.14542340053806));
#7285=CARTESIAN_POINT('Ctrl Pts',(-0.190188585522111,0.67047684793714,5.14079566989756));
#7286=CARTESIAN_POINT('Ctrl Pts',(-0.200914454344219,0.662056333977536,
5.14095167118437));
#7287=CARTESIAN_POINT('Ctrl Pts',(-0.221708714055234,0.648617241117306,
5.14525637858851));
#7288=CARTESIAN_POINT('Ctrl Pts',(-0.233167916957744,0.642702041451141,
5.14969169592803));
#7289=CARTESIAN_POINT('Ctrl Pts',(-0.255218233948888,0.63481421967861,5.16248113705728));
#7290=CARTESIAN_POINT('Ctrl Pts',(-0.265816531344893,0.63285168585486,5.17082909423827));
#7291=CARTESIAN_POINT('Ctrl Pts',(-0.283586493490155,0.63285168585486,5.18859905638354));
#7292=CARTESIAN_POINT('Ctrl Pts',(-0.291934450671145,0.63481421967861,5.19919735377954));
#7293=CARTESIAN_POINT('Ctrl Pts',(-0.304723891800398,0.642702041451141,
5.22124767077068));
#7294=CARTESIAN_POINT('Ctrl Pts',(-0.309159209139921,0.648617241117306,
5.23270687367319));
#7295=CARTESIAN_POINT('Ctrl Pts',(-0.313463916544059,0.662056333977536,
5.25350113338421));
#7296=CARTESIAN_POINT('Ctrl Pts',(-0.313619917830871,0.67047684793714,5.26422700220632));
#7297=CARTESIAN_POINT('Ctrl Pts',(-0.308992187190372,0.688564081560337,
5.28329100762279));
#7298=CARTESIAN_POINT('Ctrl Pts',(-0.30420108096549,0.698221830356238,5.29163586300025));
#7299=CARTESIAN_POINT('Ctrl Pts',(-0.291635863000248,0.715991732016857,
5.30420108096549));
#7300=CARTESIAN_POINT('Ctrl Pts',(-0.283029928759383,0.725280259543277,
5.30925326605378));
#7301=CARTESIAN_POINT('Ctrl Pts',(-0.263022185823527,0.742032846767245,
5.31482473421366));
#7302=CARTESIAN_POINT('Ctrl Pts',(-0.251627048247156,0.749506871777696,
5.31533800168111));
#7303=CARTESIAN_POINT('Ctrl Pts',(-0.229574690995115,0.761166746032619,
5.312291391818));
#7304=CARTESIAN_POINT('Ctrl Pts',(-0.21744475307808,0.766133383144486,5.308526809493));
#7305=CARTESIAN_POINT('Ctrl Pts',(-0.194447341753735,0.772681811266156,
5.29668446269695));
#7306=CARTESIAN_POINT('Ctrl Pts',(-0.183586493490155,0.774273042092169,
5.28859905638354));
#7307=CARTESIAN_POINT('Ctrl Pts',(-0.174701512417524,0.774273042092169,
5.2797140753109));
#7308=CARTESIAN_POINT('',(-0.20649711574556,0.777817459305203,5.10649711574556));
#7309=CARTESIAN_POINT('',(0.943502884254441,-0.848528137423857,6.25649711574556));
#7310=CARTESIAN_POINT('',(-0.22493035136938,0.845307347360138,5.22948523635905));
#7311=CARTESIAN_POINT('Ctrl Pts',(-0.22493035136938,0.845307347360138,5.22948523635905));
#7312=CARTESIAN_POINT('Ctrl Pts',(-0.233814216743385,0.845307347360138,
5.23836910173305));
#7313=CARTESIAN_POINT('Ctrl Pts',(-0.244662209941247,0.843699478096003,
5.24646641341103));
#7314=CARTESIAN_POINT('Ctrl Pts',(-0.267616320692928,0.837090012141717,
5.2583526832587));
#7315=CARTESIAN_POINT('Ctrl Pts',(-0.279716413955571,0.832079840080031,
5.26214850349636));
#7316=CARTESIAN_POINT('Ctrl Pts',(-0.3017133901314,0.820337643172961,5.26525283874309));
#7317=CARTESIAN_POINT('Ctrl Pts',(-0.313078704673424,0.812819819637263,
5.26476972669999));
#7318=CARTESIAN_POINT('Ctrl Pts',(-0.333043370328011,0.796006166512776,
5.25924068946332));
#7319=CARTESIAN_POINT('Ctrl Pts',(-0.34163664511408,0.786701304059523,5.25420029885166));
#7320=CARTESIAN_POINT('Ctrl Pts',(-0.354200298851658,0.768933614550881,
5.24163664511408));
#7321=CARTESIAN_POINT('Ctrl Pts',(-0.359003388103157,0.759293157295718,
5.23328067168817));
#7322=CARTESIAN_POINT('Ctrl Pts',(-0.363674622035041,0.741266387103756,
5.21417380933837));
#7323=CARTESIAN_POINT('Ctrl Pts',(-0.363549424787436,0.732888284319023,
5.20341680408705));
#7324=CARTESIAN_POINT('Ctrl Pts',(-0.359301756135174,0.719529169803534,
5.18256316131676));
#7325=CARTESIAN_POINT('Ctrl Pts',(-0.354896526024753,0.713657162034742,
5.17107247792688));
#7326=CARTESIAN_POINT('Ctrl Pts',(-0.342149933921371,0.705831016678426,
5.1489786894309));
#7327=CARTESIAN_POINT('Ctrl Pts',(-0.333814216743386,0.703885991122829,
5.13836910173305));
#7328=CARTESIAN_POINT('Ctrl Pts',(-0.316046485995375,0.703885991122829,
5.12060137098504));
#7329=CARTESIAN_POINT('Ctrl Pts',(-0.305436898297526,0.705831016678426,
5.11226565380706));
#7330=CARTESIAN_POINT('Ctrl Pts',(-0.28334310980155,0.713657162034742,5.09951906170368));
#7331=CARTESIAN_POINT('Ctrl Pts',(-0.27185242641167,0.719529169803534,5.09511383159326));
#7332=CARTESIAN_POINT('Ctrl Pts',(-0.250998783641374,0.732888284319023,
5.09086616294099));
#7333=CARTESIAN_POINT('Ctrl Pts',(-0.240241778390058,0.741266387103756,
5.09074096569339));
#7334=CARTESIAN_POINT('Ctrl Pts',(-0.221134916040255,0.759293157295718,
5.09541219962527));
#7335=CARTESIAN_POINT('Ctrl Pts',(-0.212778942614348,0.768933614550881,
5.10021528887677));
#7336=CARTESIAN_POINT('Ctrl Pts',(-0.206497115745559,0.777817459305202,
5.10649711574556));
#7337=CARTESIAN_POINT('Ctrl Pts',(-0.206497115745559,0.777817459305203,
5.10649711574556));
#7338=CARTESIAN_POINT('Ctrl Pts',(-0.200215288876771,0.786701304059523,
5.11277894261435));
#7339=CARTESIAN_POINT('Ctrl Pts',(-0.195174898265109,0.796006166512776,
5.12137221740042));
#7340=CARTESIAN_POINT('Ctrl Pts',(-0.189645861028441,0.812819819637263,
5.14133688305501));
#7341=CARTESIAN_POINT('Ctrl Pts',(-0.189162748985339,0.820337643172961,
5.15270219759703));
#7342=CARTESIAN_POINT('Ctrl Pts',(-0.192267084232068,0.832079840080031,
5.17469917377286));
#7343=CARTESIAN_POINT('Ctrl Pts',(-0.196062904469725,0.837090012141718,
5.1867992670355));
#7344=CARTESIAN_POINT('Ctrl Pts',(-0.207949174317403,0.843699478096003,
5.20975337778718));
#7345=CARTESIAN_POINT('Ctrl Pts',(-0.216046485995375,0.845307347360138,
5.22060137098504));
#7346=CARTESIAN_POINT('Ctrl Pts',(-0.22493035136938,0.845307347360138,5.22948523635905));
#7347=CARTESIAN_POINT('Origin',(3.13553390593274,-0.848528137423857,4.06446609406726));
#7348=CARTESIAN_POINT('',(3.1332564634379,-0.703885991122829,4.06218865157243));
#7349=CARTESIAN_POINT('',(3.15624458405139,-0.777817459305203,3.94375541594861));
#7350=CARTESIAN_POINT('Ctrl Pts',(3.1332564634379,-0.703885991122829,4.06218865157243));
#7351=CARTESIAN_POINT('Ctrl Pts',(3.14214032881191,-0.703885991122829,4.05330478619842));
#7352=CARTESIAN_POINT('Ctrl Pts',(3.15047604598989,-0.705831016678427,4.04269519850058));
#7353=CARTESIAN_POINT('Ctrl Pts',(3.16322263809328,-0.713657162034742,4.0206014100046));
#7354=CARTESIAN_POINT('Ctrl Pts',(3.1676278682037,-0.719529169803534,4.00911072661472));
#7355=CARTESIAN_POINT('Ctrl Pts',(3.17187553685596,-0.732888284319023,3.98825708384442));
#7356=CARTESIAN_POINT('Ctrl Pts',(3.17200073410357,-0.741266387103756,3.97750007859311));
#7357=CARTESIAN_POINT('Ctrl Pts',(3.16732950017168,-0.759293157295718,3.9583932162433));
#7358=CARTESIAN_POINT('Ctrl Pts',(3.16252641092018,-0.768933614550882,3.9500372428174));
#7359=CARTESIAN_POINT('Ctrl Pts',(3.15624458405139,-0.777817459305202,3.94375541594861));
#7360=CARTESIAN_POINT('Ctrl Pts',(3.15624458405139,-0.777817459305203,3.94375541594861));
#7361=CARTESIAN_POINT('Ctrl Pts',(3.1499627571826,-0.786701304059523,3.93747358907982));
#7362=CARTESIAN_POINT('Ctrl Pts',(3.14136948239654,-0.796006166512776,3.93243319846816));
#7363=CARTESIAN_POINT('Ctrl Pts',(3.12140481674195,-0.812819819637263,3.92690416123149));
#7364=CARTESIAN_POINT('Ctrl Pts',(3.11003950219992,-0.820337643172961,3.92642104918839));
#7365=CARTESIAN_POINT('Ctrl Pts',(3.0880425260241,-0.832079840080031,3.92952538443512));
#7366=CARTESIAN_POINT('Ctrl Pts',(3.07594243276145,-0.837090012141717,3.93332120467277));
#7367=CARTESIAN_POINT('Ctrl Pts',(3.05298832200977,-0.843699478096003,3.94520747452045));
#7368=CARTESIAN_POINT('Ctrl Pts',(3.04214032881191,-0.845307347360138,3.95330478619842));
#7369=CARTESIAN_POINT('Ctrl Pts',(3.0243725980639,-0.845307347360138,3.97107251694643));
#7370=CARTESIAN_POINT('Ctrl Pts',(3.01627528638593,-0.843699478096003,3.9819205101443));
#7371=CARTESIAN_POINT('Ctrl Pts',(3.00438901653825,-0.837090012141717,4.00487462089598));
#7372=CARTESIAN_POINT('Ctrl Pts',(3.00059319630059,-0.832079840080031,4.01697471415862));
#7373=CARTESIAN_POINT('Ctrl Pts',(2.99748886105386,-0.820337643172961,4.03897169033445));
#7374=CARTESIAN_POINT('Ctrl Pts',(2.99797197309696,-0.812819819637263,4.05033700487647));
#7375=CARTESIAN_POINT('Ctrl Pts',(3.00350101033363,-0.796006166512776,4.07030167053106));
#7376=CARTESIAN_POINT('Ctrl Pts',(3.00854140094529,-0.786701304059523,4.07889494531713));
#7377=CARTESIAN_POINT('Ctrl Pts',(3.02110505468287,-0.768933614550882,4.09145859905471));
#7378=CARTESIAN_POINT('Ctrl Pts',(3.02946102810878,-0.759293157295718,4.09626168830621));
#7379=CARTESIAN_POINT('Ctrl Pts',(3.04856789045858,-0.741266387103756,4.10093292223809));
#7380=CARTESIAN_POINT('Ctrl Pts',(3.0593248957099,-0.732888284319023,4.10080772499049));
#7381=CARTESIAN_POINT('Ctrl Pts',(3.08017853848019,-0.719529169803534,4.09656005633822));
#7382=CARTESIAN_POINT('Ctrl Pts',(3.09166922187007,-0.713657162034742,4.0921548262278));
#7383=CARTESIAN_POINT('Ctrl Pts',(3.11376301036605,-0.705831016678427,4.07940823412442));
#7384=CARTESIAN_POINT('Ctrl Pts',(3.1243725980639,-0.703885991122829,4.07107251694644));
#7385=CARTESIAN_POINT('Ctrl Pts',(3.1332564634379,-0.703885991122829,4.06218865157243));
#7386=CARTESIAN_POINT('',(3.10624458405139,-0.707106781186548,3.89375541594861));
#7387=CARTESIAN_POINT('',(3.20624458405139,-0.848528137423857,3.99375541594861));
#7388=CARTESIAN_POINT('',(3.08302762448605,-0.63285168585486,4.01195981262057));
#7389=CARTESIAN_POINT('Ctrl Pts',(3.08302762448605,-0.63285168585486,4.01195981262057));
#7390=CARTESIAN_POINT('Ctrl Pts',(3.07414264341342,-0.63285168585486,4.0208447936932));
#7391=CARTESIAN_POINT('Ctrl Pts',(3.06354434601741,-0.634814219678611,4.02919275087419));
#7392=CARTESIAN_POINT('Ctrl Pts',(3.04149402902627,-0.642702041451141,4.04198219200345));
#7393=CARTESIAN_POINT('Ctrl Pts',(3.03003482612376,-0.648617241117307,4.04641750934297));
#7394=CARTESIAN_POINT('Ctrl Pts',(3.00924056641274,-0.662056333977536,4.05072221674711));
#7395=CARTESIAN_POINT('Ctrl Pts',(2.99851469759064,-0.67047684793714,4.05087821803392));
#7396=CARTESIAN_POINT('Ctrl Pts',(2.97945069217416,-0.688564081560337,4.04625048739342));
#7397=CARTESIAN_POINT('Ctrl Pts',(2.9711058367967,-0.698221830356238,4.04145938116854));
#7398=CARTESIAN_POINT('Ctrl Pts',(2.95854061883146,-0.715991732016857,4.0288941632033));
#7399=CARTESIAN_POINT('Ctrl Pts',(2.95348843374317,-0.725280259543277,4.02028822896243));
#7400=CARTESIAN_POINT('Ctrl Pts',(2.94791696558329,-0.742032846767244,4.00028048602658));
#7401=CARTESIAN_POINT('Ctrl Pts',(2.94740369811584,-0.749506871777695,3.9888853484502));
#7402=CARTESIAN_POINT('Ctrl Pts',(2.95045030797895,-0.761166746032619,3.96683299119816));
#7403=CARTESIAN_POINT('Ctrl Pts',(2.95421489030395,-0.766133383144486,3.95470305328113));
#7404=CARTESIAN_POINT('Ctrl Pts',(2.9660572371,-0.772681811266156,3.93170564195678));
#7405=CARTESIAN_POINT('Ctrl Pts',(2.97414264341342,-0.774273042092169,3.9208447936932));
#7406=CARTESIAN_POINT('Ctrl Pts',(2.99191260555868,-0.774273042092169,3.90307483154794));
#7407=CARTESIAN_POINT('Ctrl Pts',(3.00277345382226,-0.772681811266156,3.89498942523453));
#7408=CARTESIAN_POINT('Ctrl Pts',(3.0257708651466,-0.766133383144485,3.88314707843848));
#7409=CARTESIAN_POINT('Ctrl Pts',(3.03790080306364,-0.761166746032619,3.87938249611348));
#7410=CARTESIAN_POINT('Ctrl Pts',(3.05995316031568,-0.749506871777695,3.87633588625036));
#7411=CARTESIAN_POINT('Ctrl Pts',(3.07134829789205,-0.742032846767244,3.87684915371782));
#7412=CARTESIAN_POINT('Ctrl Pts',(3.09135604082791,-0.725280259543277,3.8824206218777));
#7413=CARTESIAN_POINT('Ctrl Pts',(3.09996197506877,-0.715991732016857,3.88747280696599));
#7414=CARTESIAN_POINT('Ctrl Pts',(3.10624458405139,-0.707106781186548,3.89375541594861));
#7415=CARTESIAN_POINT('Ctrl Pts',(3.10624458405139,-0.707106781186548,3.89375541594861));
#7416=CARTESIAN_POINT('Ctrl Pts',(3.11252719303401,-0.698221830356238,3.90003802493123));
#7417=CARTESIAN_POINT('Ctrl Pts',(3.1173182992589,-0.688564081560337,3.90838288030869));
#7418=CARTESIAN_POINT('Ctrl Pts',(3.1219460298994,-0.67047684793714,3.92744688572516));
#7419=CARTESIAN_POINT('Ctrl Pts',(3.12179002861258,-0.662056333977536,3.93817275454727));
#7420=CARTESIAN_POINT('Ctrl Pts',(3.11748532120845,-0.648617241117307,3.95896701425828));
#7421=CARTESIAN_POINT('Ctrl Pts',(3.11305000386892,-0.642702041451141,3.97042621716079));
#7422=CARTESIAN_POINT('Ctrl Pts',(3.10026056273967,-0.634814219678611,3.99247653415194));
#7423=CARTESIAN_POINT('Ctrl Pts',(3.09191260555868,-0.63285168585486,4.00307483154794));
#7424=CARTESIAN_POINT('Ctrl Pts',(3.08302762448605,-0.63285168585486,4.01195981262057));
#7425=CARTESIAN_POINT('Origin',(3.13553390593274,-0.848528137423857,4.06446609406726));
#7426=CARTESIAN_POINT('',(2.08804018737943,0.774273042092169,3.01697237551395));
#7427=CARTESIAN_POINT('',(2.10624458405139,0.707106781186547,2.89375541594861));
#7428=CARTESIAN_POINT('Ctrl Pts',(2.08804018737943,0.774273042092169,3.01697237551395));
#7429=CARTESIAN_POINT('Ctrl Pts',(2.09692516845206,0.774273042092169,3.00808739444132));
#7430=CARTESIAN_POINT('Ctrl Pts',(2.10501057476547,0.772681811266156,2.99722654617774));
#7431=CARTESIAN_POINT('Ctrl Pts',(2.11685292156153,0.766133383144486,2.9742291348534));
#7432=CARTESIAN_POINT('Ctrl Pts',(2.12061750388653,0.76116674603262,2.96209919693636));
#7433=CARTESIAN_POINT('Ctrl Pts',(2.12366411374964,0.749506871777696,2.94004683968432));
#7434=CARTESIAN_POINT('Ctrl Pts',(2.12315084628218,0.742032846767244,2.92865170210795));
#7435=CARTESIAN_POINT('Ctrl Pts',(2.1175793781223,0.725280259543277,2.90864395917209));
#7436=CARTESIAN_POINT('Ctrl Pts',(2.11252719303401,0.715991732016857,2.90003802493123));
#7437=CARTESIAN_POINT('Ctrl Pts',(2.10624458405139,0.707106781186547,2.89375541594861));
#7438=CARTESIAN_POINT('Ctrl Pts',(2.10624458405139,0.707106781186548,2.89375541594861));
#7439=CARTESIAN_POINT('Ctrl Pts',(2.09996197506877,0.698221830356238,2.88747280696599));
#7440=CARTESIAN_POINT('Ctrl Pts',(2.09161711969131,0.688564081560337,2.8826817007411));
#7441=CARTESIAN_POINT('Ctrl Pts',(2.07255311427484,0.67047684793714,2.87805397010061));
#7442=CARTESIAN_POINT('Ctrl Pts',(2.06182724545273,0.662056333977536,2.87820997138742));
#7443=CARTESIAN_POINT('Ctrl Pts',(2.04103298574172,0.648617241117307,2.88251467879155));
#7444=CARTESIAN_POINT('Ctrl Pts',(2.02957378283921,0.642702041451141,2.88694999613108));
#7445=CARTESIAN_POINT('Ctrl Pts',(2.00752346584806,0.634814219678611,2.89973943726033));
#7446=CARTESIAN_POINT('Ctrl Pts',(1.99692516845206,0.63285168585486,2.90808739444132));
#7447=CARTESIAN_POINT('Ctrl Pts',(1.9791552063068,0.63285168585486,2.92585735658658));
#7448=CARTESIAN_POINT('Ctrl Pts',(1.97080724912581,0.634814219678611,2.93645565398259));
#7449=CARTESIAN_POINT('Ctrl Pts',(1.95801780799655,0.642702041451141,2.95850597097373));
#7450=CARTESIAN_POINT('Ctrl Pts',(1.95358249065703,0.648617241117307,2.96996517387624));
#7451=CARTESIAN_POINT('Ctrl Pts',(1.94927778325289,0.662056333977536,2.99075943358726));
#7452=CARTESIAN_POINT('Ctrl Pts',(1.94912178196608,0.67047684793714,3.00148530240937));
#7453=CARTESIAN_POINT('Ctrl Pts',(1.95374951260658,0.688564081560337,3.02054930782584));
#7454=CARTESIAN_POINT('Ctrl Pts',(1.95854061883146,0.698221830356238,3.0288941632033));
#7455=CARTESIAN_POINT('Ctrl Pts',(1.9711058367967,0.715991732016857,3.04145938116854));
#7456=CARTESIAN_POINT('Ctrl Pts',(1.97971177103757,0.725280259543277,3.04651156625683));
#7457=CARTESIAN_POINT('Ctrl Pts',(1.99971951397343,0.742032846767244,3.05208303441671));
#7458=CARTESIAN_POINT('Ctrl Pts',(2.0111146515498,0.749506871777696,3.05259630188416));
#7459=CARTESIAN_POINT('Ctrl Pts',(2.03316700880184,0.76116674603262,3.04954969202105));
#7460=CARTESIAN_POINT('Ctrl Pts',(2.04529694671887,0.766133383144486,3.04578510969605));
#7461=CARTESIAN_POINT('Ctrl Pts',(2.06829435804322,0.772681811266156,3.0339427629));
#7462=CARTESIAN_POINT('Ctrl Pts',(2.0791552063068,0.774273042092169,3.02585735658658));
#7463=CARTESIAN_POINT('Ctrl Pts',(2.08804018737943,0.774273042092169,3.01697237551395));
#7464=CARTESIAN_POINT('',(2.05624458405139,0.777817459305202,2.84375541594861));
#7465=CARTESIAN_POINT('',(3.20624458405139,-0.848528137423857,3.99375541594861));
#7466=CARTESIAN_POINT('',(2.03781134842757,0.845307347360138,2.9667435365621));
#7467=CARTESIAN_POINT('Ctrl Pts',(2.03781134842757,0.845307347360138,2.9667435365621));
#7468=CARTESIAN_POINT('Ctrl Pts',(2.02892748305357,0.845307347360138,2.9756274019361));
#7469=CARTESIAN_POINT('Ctrl Pts',(2.01807948985571,0.843699478096003,2.98372471361407));
#7470=CARTESIAN_POINT('Ctrl Pts',(1.99512537910402,0.837090012141717,2.99561098346175));
#7471=CARTESIAN_POINT('Ctrl Pts',(1.98302528584138,0.832079840080031,2.99940680369941));
#7472=CARTESIAN_POINT('Ctrl Pts',(1.96102830966555,0.820337643172961,3.00251113894614));
#7473=CARTESIAN_POINT('Ctrl Pts',(1.94966299512353,0.812819819637263,3.00202802690304));
#7474=CARTESIAN_POINT('Ctrl Pts',(1.92969832946894,0.796006166512776,2.99649898966637));
#7475=CARTESIAN_POINT('Ctrl Pts',(1.92110505468287,0.786701304059523,2.99145859905471));
#7476=CARTESIAN_POINT('Ctrl Pts',(1.9085414009453,0.768933614550882,2.97889494531713));
#7477=CARTESIAN_POINT('Ctrl Pts',(1.9037383116938,0.759293157295718,2.97053897189122));
#7478=CARTESIAN_POINT('Ctrl Pts',(1.89906707776191,0.741266387103756,2.95143210954142));
#7479=CARTESIAN_POINT('Ctrl Pts',(1.89919227500952,0.732888284319023,2.9406751042901));
#7480=CARTESIAN_POINT('Ctrl Pts',(1.90343994366178,0.719529169803535,2.91982146151981));
#7481=CARTESIAN_POINT('Ctrl Pts',(1.9078451737722,0.713657162034741,2.90833077812993));
#7482=CARTESIAN_POINT('Ctrl Pts',(1.92059176587558,0.705831016678426,2.88623698963395));
#7483=CARTESIAN_POINT('Ctrl Pts',(1.92892748305357,0.703885991122829,2.8756274019361));
#7484=CARTESIAN_POINT('Ctrl Pts',(1.94669521380158,0.703885991122829,2.85785967118809));
#7485=CARTESIAN_POINT('Ctrl Pts',(1.95730480149943,0.705831016678427,2.84952395401011));
#7486=CARTESIAN_POINT('Ctrl Pts',(1.9793985899954,0.713657162034743,2.83677736190672));
#7487=CARTESIAN_POINT('Ctrl Pts',(1.99088927338528,0.719529169803534,2.8323721317963));
#7488=CARTESIAN_POINT('Ctrl Pts',(2.01174291615558,0.732888284319023,2.82812446314404));
#7489=CARTESIAN_POINT('Ctrl Pts',(2.0224999214069,0.741266387103756,2.82799926589644));
#7490=CARTESIAN_POINT('Ctrl Pts',(2.0416067837567,0.759293157295718,2.83267049982832));
#7491=CARTESIAN_POINT('Ctrl Pts',(2.0499627571826,0.768933614550881,2.83747358907982));
#7492=CARTESIAN_POINT('Ctrl Pts',(2.05624458405139,0.777817459305202,2.84375541594861));
#7493=CARTESIAN_POINT('Ctrl Pts',(2.05624458405139,0.777817459305202,2.84375541594861));
#7494=CARTESIAN_POINT('Ctrl Pts',(2.06252641092018,0.786701304059523,2.8500372428174));
#7495=CARTESIAN_POINT('Ctrl Pts',(2.06756680153184,0.796006166512776,2.85863051760347));
#7496=CARTESIAN_POINT('Ctrl Pts',(2.07309583876851,0.812819819637263,2.87859518325805));
#7497=CARTESIAN_POINT('Ctrl Pts',(2.07357895081161,0.820337643172961,2.88996049780008));
#7498=CARTESIAN_POINT('Ctrl Pts',(2.07047461556488,0.832079840080031,2.9119574739759));
#7499=CARTESIAN_POINT('Ctrl Pts',(2.06667879532723,0.837090012141717,2.92405756723855));
#7500=CARTESIAN_POINT('Ctrl Pts',(2.05479252547955,0.843699478096003,2.94701167799023));
#7501=CARTESIAN_POINT('Ctrl Pts',(2.04669521380158,0.845307347360138,2.95785967118809));
#7502=CARTESIAN_POINT('Ctrl Pts',(2.03781134842757,0.845307347360138,2.9667435365621));
#7503=CARTESIAN_POINT('Origin',(3.94974746830583,0.,3.74730880654188));
#7504=CARTESIAN_POINT('',(3.87581600012346,0.0999999999999996,3.67337733835951));
#7505=CARTESIAN_POINT('',(3.94974746830583,-1.22464679914735E-17,3.60588745030457));
#7506=CARTESIAN_POINT('Ctrl Pts',(3.87581600012346,0.0999999999999996,3.67337733835951));
#7507=CARTESIAN_POINT('Ctrl Pts',(3.88469986549747,0.0999999999999996,3.6644934729855));
#7508=CARTESIAN_POINT('Ctrl Pts',(3.89434109608111,0.0974877239801237,3.65518939869332));
#7509=CARTESIAN_POINT('Ctrl Pts',(3.91236962608181,0.0872802053318249,3.63837754809465));
#7510=CARTESIAN_POINT('Ctrl Pts',(3.92074850068551,0.0795853421796018,3.63086050919806));
#7511=CARTESIAN_POINT('Ctrl Pts',(3.934107615201,0.0618360346560355,3.61911831229099));
#7512=CARTESIAN_POINT('Ctrl Pts',(3.93997885607498,0.0505959173616165,3.61410735066604));
#7513=CARTESIAN_POINT('Ctrl Pts',(3.94780322881767,0.025960017775146,3.60749609499082));
#7514=CARTESIAN_POINT('Ctrl Pts',(3.94974746830583,0.0125636537375776,3.60588745030457));
#7515=CARTESIAN_POINT('Ctrl Pts',(3.94974746830583,-2.08166817117217E-17,
3.60588745030457));
#7516=CARTESIAN_POINT('',(3.80832611206852,-8.64375321888493E-17,3.74730880654188));
#7517=CARTESIAN_POINT('Ctrl Pts',(3.80832611206852,-3.81639164714898E-17,
3.74730880654188));
#7518=CARTESIAN_POINT('Ctrl Pts',(3.80832611206852,0.0125636537375776,3.74730880654188));
#7519=CARTESIAN_POINT('Ctrl Pts',(3.80993475675477,0.025960017775146,3.74536456705372));
#7520=CARTESIAN_POINT('Ctrl Pts',(3.81654601243,0.0505959173616165,3.73754019431103));
#7521=CARTESIAN_POINT('Ctrl Pts',(3.82155697405494,0.0618360346560354,3.73166895343705));
#7522=CARTESIAN_POINT('Ctrl Pts',(3.83329917096201,0.0795853421796018,3.71830983892156));
#7523=CARTESIAN_POINT('Ctrl Pts',(3.8408162098586,0.087280205331825,3.70993096431786));
#7524=CARTESIAN_POINT('Ctrl Pts',(3.85762806045727,0.0974877239801237,3.69190243431716));
#7525=CARTESIAN_POINT('Ctrl Pts',(3.86693213474945,0.0999999999999996,3.68226120373351));
#7526=CARTESIAN_POINT('Ctrl Pts',(3.87581600012346,0.0999999999999996,3.67337733835951));
#7527=CARTESIAN_POINT('Ctrl Pts',(3.94974746830583,1.73472347597681E-17,
3.60588745030457));
#7528=CARTESIAN_POINT('Ctrl Pts',(3.94974746830583,-0.0125636537375776,
3.60588745030457));
#7529=CARTESIAN_POINT('Ctrl Pts',(3.94780322881767,-0.0259600177751452,
3.60749609499082));
#7530=CARTESIAN_POINT('Ctrl Pts',(3.93997885607498,-0.0505959173616158,
3.61410735066604));
#7531=CARTESIAN_POINT('Ctrl Pts',(3.934107615201,-0.0618360346560354,3.61911831229099));
#7532=CARTESIAN_POINT('Ctrl Pts',(3.92074850068551,-0.0795853421796018,
3.63086050919806));
#7533=CARTESIAN_POINT('Ctrl Pts',(3.91236962608181,-0.0872802053318244,
3.63837754809465));
#7534=CARTESIAN_POINT('Ctrl Pts',(3.89434109608111,-0.0974877239801237,
3.65518939869332));
#7535=CARTESIAN_POINT('Ctrl Pts',(3.88469986549747,-0.0999999999999996,
3.6644934729855));
#7536=CARTESIAN_POINT('Ctrl Pts',(3.86693213474945,-0.0999999999999996,
3.68226120373351));
#7537=CARTESIAN_POINT('Ctrl Pts',(3.85762806045727,-0.097487723980124,3.69190243431716));
#7538=CARTESIAN_POINT('Ctrl Pts',(3.8408162098586,-0.0872802053318249,3.70993096431786));
#7539=CARTESIAN_POINT('Ctrl Pts',(3.83329917096201,-0.0795853421796018,
3.71830983892156));
#7540=CARTESIAN_POINT('Ctrl Pts',(3.82155697405494,-0.0618360346560355,
3.73166895343705));
#7541=CARTESIAN_POINT('Ctrl Pts',(3.81654601243,-0.0505959173616168,3.73754019431103));
#7542=CARTESIAN_POINT('Ctrl Pts',(3.80993475675477,-0.0259600177751463,
3.74536456705372));
#7543=CARTESIAN_POINT('Ctrl Pts',(3.80832611206852,-0.0125636537375776,
3.74730880654188));
#7544=CARTESIAN_POINT('Ctrl Pts',(3.80832611206852,-6.24500451351651E-17,
3.74730880654188));
#7545=CARTESIAN_POINT('',(3.87903679018718,-2.00010218035512E-17,3.53517677218592));
#7546=CARTESIAN_POINT('',(4.02045814642449,-1.22464679914735E-17,3.67659812842323));
#7547=CARTESIAN_POINT('',(3.73761543394987,-7.16406808132285E-17,3.67659812842323));
#7548=CARTESIAN_POINT('Ctrl Pts',(3.73761543394987,-2.42861286636753E-17,
3.67659812842323));
#7549=CARTESIAN_POINT('Ctrl Pts',(3.73761543394987,-0.0125652179652416,
3.67659812842323));
#7550=CARTESIAN_POINT('Ctrl Pts',(3.73920769789142,-0.0259622584309892,
3.6746366432122));
#7551=CARTESIAN_POINT('Ctrl Pts',(3.74575851207979,-0.0505977320073435,
3.6667511826246));
#7552=CARTESIAN_POINT('Ctrl Pts',(3.75072620265967,-0.0618368682969031,
3.66083700309556));
#7553=CARTESIAN_POINT('Ctrl Pts',(3.7623860769146,-0.0795845181448063,3.64739791023533));
#7554=CARTESIAN_POINT('Ctrl Pts',(3.76985905575846,-0.0872791387223183,
3.63897636883716));
#7555=CARTESIAN_POINT('Ctrl Pts',(3.78660923799323,-0.0974871089174108,
3.62088679295154));
#7556=CARTESIAN_POINT('Ctrl Pts',(3.79589671378286,-0.0999999999999996,
3.61122801416417));
#7557=CARTESIAN_POINT('Ctrl Pts',(3.81366667592812,-0.0999999999999996,
3.59345805201891));
#7558=CARTESIAN_POINT('Ctrl Pts',(3.82332545471549,-0.0974871089174108,
3.58417057622928));
#7559=CARTESIAN_POINT('Ctrl Pts',(3.84141503060112,-0.0872791387223183,
3.56742039399451));
#7560=CARTESIAN_POINT('Ctrl Pts',(3.84983657199928,-0.0795845181448063,
3.55994741515065));
#7561=CARTESIAN_POINT('Ctrl Pts',(3.86327566485951,-0.0618368682969031,
3.54828754089572));
#7562=CARTESIAN_POINT('Ctrl Pts',(3.86918984438855,-0.0505977320073432,
3.54331985031584));
#7563=CARTESIAN_POINT('Ctrl Pts',(3.87707530497615,-0.025962258430989,3.53676903612747));
#7564=CARTESIAN_POINT('Ctrl Pts',(3.87903679018718,-0.0125652179652416,
3.53517677218592));
#7565=CARTESIAN_POINT('Ctrl Pts',(3.87903679018718,1.73472347597681E-17,
3.53517677218592));
#7566=CARTESIAN_POINT('',(3.80478169485549,0.0999999999999998,3.60234303309154));
#7567=CARTESIAN_POINT('Ctrl Pts',(3.80478169485549,0.0999999999999996,3.60234303309154));
#7568=CARTESIAN_POINT('Ctrl Pts',(3.79589671378286,0.0999999999999996,3.61122801416417));
#7569=CARTESIAN_POINT('Ctrl Pts',(3.78660923799323,0.0974871089174108,3.62088679295154));
#7570=CARTESIAN_POINT('Ctrl Pts',(3.76985905575846,0.0872791387223183,3.63897636883716));
#7571=CARTESIAN_POINT('Ctrl Pts',(3.7623860769146,0.0795845181448063,3.64739791023533));
#7572=CARTESIAN_POINT('Ctrl Pts',(3.75072620265967,0.0618368682969031,3.66083700309556));
#7573=CARTESIAN_POINT('Ctrl Pts',(3.74575851207979,0.0505977320073435,3.6667511826246));
#7574=CARTESIAN_POINT('Ctrl Pts',(3.73920769789142,0.0259622584309889,3.6746366432122));
#7575=CARTESIAN_POINT('Ctrl Pts',(3.73761543394987,0.0125652179652416,3.67659812842323));
#7576=CARTESIAN_POINT('Ctrl Pts',(3.73761543394987,2.42861286636753E-17,
3.67659812842323));
#7577=CARTESIAN_POINT('Ctrl Pts',(3.87903679018718,-1.38777878078145E-17,
3.53517677218592));
#7578=CARTESIAN_POINT('Ctrl Pts',(3.87903679018718,0.0125652179652416,3.53517677218592));
#7579=CARTESIAN_POINT('Ctrl Pts',(3.87707530497615,0.0259622584309889,3.53676903612747));
#7580=CARTESIAN_POINT('Ctrl Pts',(3.86918984438855,0.0505977320073435,3.54331985031584));
#7581=CARTESIAN_POINT('Ctrl Pts',(3.86327566485951,0.0618368682969031,3.54828754089572));
#7582=CARTESIAN_POINT('Ctrl Pts',(3.84983657199928,0.0795845181448063,3.55994741515065));
#7583=CARTESIAN_POINT('Ctrl Pts',(3.84141503060112,0.0872791387223183,3.56742039399451));
#7584=CARTESIAN_POINT('Ctrl Pts',(3.82332545471549,0.0974871089174108,3.58417057622928));
#7585=CARTESIAN_POINT('Ctrl Pts',(3.81366667592812,0.0999999999999997,3.59345805201891));
#7586=CARTESIAN_POINT('Ctrl Pts',(3.80478169485549,0.0999999999999996,3.60234303309154));
#7587=CARTESIAN_POINT('Origin',(3.94974746830583,0.,3.74730880654188));
#7588=CARTESIAN_POINT('',(2.39765696690846,0.0999999999999997,2.19521830514451));
#7589=CARTESIAN_POINT('',(2.46482322781408,-1.13274044236671E-17,2.12096320981282));
#7590=CARTESIAN_POINT('Ctrl Pts',(2.39765696690846,0.0999999999999996,2.19521830514451));
#7591=CARTESIAN_POINT('Ctrl Pts',(2.40654194798109,0.0999999999999997,2.18633332407188));
#7592=CARTESIAN_POINT('Ctrl Pts',(2.41582942377072,0.0974871089174108,2.17667454528451));
#7593=CARTESIAN_POINT('Ctrl Pts',(2.43257960600549,0.0872791387223183,2.15858496939889));
#7594=CARTESIAN_POINT('Ctrl Pts',(2.44005258484936,0.0795845181448063,2.15016342800072));
#7595=CARTESIAN_POINT('Ctrl Pts',(2.45171245910428,0.0618368682969031,2.13672433514049));
#7596=CARTESIAN_POINT('Ctrl Pts',(2.45668014968416,0.0505977320073435,2.13081015561145));
#7597=CARTESIAN_POINT('Ctrl Pts',(2.46323096387254,0.0259622584309889,2.12292469502385));
#7598=CARTESIAN_POINT('Ctrl Pts',(2.46482322781408,0.0125652179652416,2.12096320981282));
#7599=CARTESIAN_POINT('Ctrl Pts',(2.46482322781408,-1.38777878078145E-17,
2.12096320981282));
#7600=CARTESIAN_POINT('Ctrl Pts',(2.46482322781408,-1.73472347597681E-17,
2.12096320981282));
#7601=CARTESIAN_POINT('Ctrl Pts',(2.46482322781408,-0.0125652179652416,
2.12096320981282));
#7602=CARTESIAN_POINT('Ctrl Pts',(2.46323096387254,-0.0259622584309888,
2.12292469502385));
#7603=CARTESIAN_POINT('Ctrl Pts',(2.45668014968416,-0.0505977320073434,
2.13081015561145));
#7604=CARTESIAN_POINT('Ctrl Pts',(2.45171245910428,-0.0618368682969031,
2.13672433514049));
#7605=CARTESIAN_POINT('Ctrl Pts',(2.44005258484936,-0.0795845181448063,
2.15016342800072));
#7606=CARTESIAN_POINT('Ctrl Pts',(2.43257960600549,-0.0872791387223169,
2.15858496939888));
#7607=CARTESIAN_POINT('Ctrl Pts',(2.41582942377072,-0.0974871089174101,
2.17667454528451));
#7608=CARTESIAN_POINT('Ctrl Pts',(2.40654194798109,-0.0999999999999996,
2.18633332407188));
#7609=CARTESIAN_POINT('Ctrl Pts',(2.38877198583583,-0.0999999999999996,
2.20410328621714));
#7610=CARTESIAN_POINT('Ctrl Pts',(2.37911320704846,-0.0974871089174108,
2.21339076200677));
#7611=CARTESIAN_POINT('Ctrl Pts',(2.36102363116284,-0.0872791387223183,
2.23014094424154));
#7612=CARTESIAN_POINT('Ctrl Pts',(2.35260208976467,-0.0795845181448063,
2.23761392308541));
#7613=CARTESIAN_POINT('Ctrl Pts',(2.33916299690444,-0.0618368682969031,
2.24927379734033));
#7614=CARTESIAN_POINT('Ctrl Pts',(2.3332488173754,-0.0505977320073435,2.25424148792021));
#7615=CARTESIAN_POINT('Ctrl Pts',(2.3253633567878,-0.0259622584309889,2.26079230210858));
#7616=CARTESIAN_POINT('Ctrl Pts',(2.32340187157677,-0.0125652179652416,
2.26238456605013));
#7617=CARTESIAN_POINT('Ctrl Pts',(2.32340187157677,0.0125652179652416,2.26238456605013));
#7618=CARTESIAN_POINT('Ctrl Pts',(2.3253633567878,0.0259622584309889,2.26079230210858));
#7619=CARTESIAN_POINT('Ctrl Pts',(2.3332488173754,0.0505977320073435,2.25424148792021));
#7620=CARTESIAN_POINT('Ctrl Pts',(2.33916299690444,0.0618368682969031,2.24927379734033));
#7621=CARTESIAN_POINT('Ctrl Pts',(2.35260208976467,0.0795845181448063,2.23761392308541));
#7622=CARTESIAN_POINT('Ctrl Pts',(2.36102363116284,0.0872791387223183,2.23014094424154));
#7623=CARTESIAN_POINT('Ctrl Pts',(2.37911320704846,0.0974871089174108,2.21339076200677));
#7624=CARTESIAN_POINT('Ctrl Pts',(2.38877198583583,0.0999999999999996,2.20410328621714));
#7625=CARTESIAN_POINT('Ctrl Pts',(2.39765696690846,0.0999999999999997,2.19521830514451));
#7626=CARTESIAN_POINT('',(2.39411254969543,-1.22464679914735E-17,2.05025253169417));
#7627=CARTESIAN_POINT('',(4.02045814642449,-1.22464679914735E-17,3.67659812842323));
#7628=CARTESIAN_POINT('',(2.32662266164049,0.0999999999999997,2.12418399987654));
#7629=CARTESIAN_POINT('Ctrl Pts',(2.32662266164049,0.0999999999999997,2.12418399987654));
#7630=CARTESIAN_POINT('Ctrl Pts',(2.31773879626649,0.0999999999999996,2.13306786525055));
#7631=CARTESIAN_POINT('Ctrl Pts',(2.30809756568284,0.0974877239801237,2.14237193954273));
#7632=CARTESIAN_POINT('Ctrl Pts',(2.29006903568215,0.0872802053318249,2.1591837901414));
#7633=CARTESIAN_POINT('Ctrl Pts',(2.28169016107844,0.0795853421796018,2.16670082903799));
#7634=CARTESIAN_POINT('Ctrl Pts',(2.26833104656295,0.0618360346560354,2.17844302594506));
#7635=CARTESIAN_POINT('Ctrl Pts',(2.26245980568898,0.0505959173616165,2.18345398757001));
#7636=CARTESIAN_POINT('Ctrl Pts',(2.25463543294628,0.025960017775146,2.19006524324523));
#7637=CARTESIAN_POINT('Ctrl Pts',(2.25269119345812,0.0125636537375776,2.19167388793148));
#7638=CARTESIAN_POINT('Ctrl Pts',(2.25269119345812,-0.0125636537375776,
2.19167388793148));
#7639=CARTESIAN_POINT('Ctrl Pts',(2.25463543294628,-0.0259600177751461,
2.19006524324523));
#7640=CARTESIAN_POINT('Ctrl Pts',(2.26245980568898,-0.0505959173616165,
2.18345398757001));
#7641=CARTESIAN_POINT('Ctrl Pts',(2.26833104656295,-0.0618360346560355,
2.17844302594506));
#7642=CARTESIAN_POINT('Ctrl Pts',(2.28169016107844,-0.0795853421796018,
2.16670082903799));
#7643=CARTESIAN_POINT('Ctrl Pts',(2.29006903568215,-0.087280205331825,2.1591837901414));
#7644=CARTESIAN_POINT('Ctrl Pts',(2.30809756568284,-0.097487723980124,2.14237193954273));
#7645=CARTESIAN_POINT('Ctrl Pts',(2.31773879626649,-0.0999999999999996,
2.13306786525055));
#7646=CARTESIAN_POINT('Ctrl Pts',(2.3355065270145,-0.0999999999999996,2.11530013450254));
#7647=CARTESIAN_POINT('Ctrl Pts',(2.34481060130668,-0.0974877239801237,
2.10565890391889));
#7648=CARTESIAN_POINT('Ctrl Pts',(2.36162245190535,-0.0872802053318249,
2.08763037391819));
#7649=CARTESIAN_POINT('Ctrl Pts',(2.36913949080195,-0.0795853421796018,
2.07925149931449));
#7650=CARTESIAN_POINT('Ctrl Pts',(2.38088168770902,-0.0618360346560354,
2.065892384799));
#7651=CARTESIAN_POINT('Ctrl Pts',(2.38589264933396,-0.0505959173616158,
2.06002114392502));
#7652=CARTESIAN_POINT('Ctrl Pts',(2.39250390500918,-0.0259600177751451,
2.05219677118233));
#7653=CARTESIAN_POINT('Ctrl Pts',(2.39411254969543,-0.0125636537375776,
2.05025253169417));
#7654=CARTESIAN_POINT('Ctrl Pts',(2.39411254969543,1.38777878078145E-17,
2.05025253169417));
#7655=CARTESIAN_POINT('Ctrl Pts',(2.39411254969543,2.42861286636753E-17,
2.05025253169417));
#7656=CARTESIAN_POINT('Ctrl Pts',(2.39411254969543,0.0125636537375776,2.05025253169417));
#7657=CARTESIAN_POINT('Ctrl Pts',(2.39250390500918,0.025960017775146,2.05219677118233));
#7658=CARTESIAN_POINT('Ctrl Pts',(2.38589264933396,0.0505959173616165,2.06002114392502));
#7659=CARTESIAN_POINT('Ctrl Pts',(2.38088168770902,0.0618360346560355,2.065892384799));
#7660=CARTESIAN_POINT('Ctrl Pts',(2.36913949080194,0.0795853421796018,2.07925149931449));
#7661=CARTESIAN_POINT('Ctrl Pts',(2.36162245190535,0.087280205331825,2.08763037391819));
#7662=CARTESIAN_POINT('Ctrl Pts',(2.34481060130668,0.0974877239801237,2.10565890391889));
#7663=CARTESIAN_POINT('Ctrl Pts',(2.3355065270145,0.0999999999999997,2.11530013450254));
#7664=CARTESIAN_POINT('Ctrl Pts',(2.32662266164049,0.0999999999999996,2.12418399987654));
#7665=CARTESIAN_POINT('Origin',(2.81837661840736,0.,4.87867965644036));
#7666=CARTESIAN_POINT('',(2.74444515022498,0.0999999999999997,4.80474818825798));
#7667=CARTESIAN_POINT('',(2.81837661840736,-1.22464679914735E-17,4.73725830020305));
#7668=CARTESIAN_POINT('Ctrl Pts',(2.74444515022498,0.0999999999999997,4.80474818825798));
#7669=CARTESIAN_POINT('Ctrl Pts',(2.75332901559899,0.0999999999999996,4.79586432288398));
#7670=CARTESIAN_POINT('Ctrl Pts',(2.76297024618264,0.0974877239801236,4.78656024859179));
#7671=CARTESIAN_POINT('Ctrl Pts',(2.78099877618333,0.0872802053318249,4.76974839799313));
#7672=CARTESIAN_POINT('Ctrl Pts',(2.78937765078703,0.0795853421796016,4.76223135909653));
#7673=CARTESIAN_POINT('Ctrl Pts',(2.80273676530252,0.0618360346560355,4.75048916218946));
#7674=CARTESIAN_POINT('Ctrl Pts',(2.8086080061765,0.0505959173616169,4.74547820056452));
#7675=CARTESIAN_POINT('Ctrl Pts',(2.8164323789192,0.0259600177751461,4.7388669448893));
#7676=CARTESIAN_POINT('Ctrl Pts',(2.81837661840736,0.0125636537375776,4.73725830020305));
#7677=CARTESIAN_POINT('Ctrl Pts',(2.81837661840736,-3.81639164714898E-17,
4.73725830020305));
#7678=CARTESIAN_POINT('',(2.67695526217005,-9.68458730447102E-17,4.87867965644036));
#7679=CARTESIAN_POINT('Ctrl Pts',(2.67695526217005,-6.93889390390723E-17,
4.87867965644036));
#7680=CARTESIAN_POINT('Ctrl Pts',(2.67695526217005,0.0125636537375775,4.87867965644036));
#7681=CARTESIAN_POINT('Ctrl Pts',(2.6785639068563,0.025960017775146,4.8767354169522));
#7682=CARTESIAN_POINT('Ctrl Pts',(2.68517516253152,0.0505959173616165,4.8689110442095));
#7683=CARTESIAN_POINT('Ctrl Pts',(2.69018612415646,0.0618360346560354,4.86303980333552));
#7684=CARTESIAN_POINT('Ctrl Pts',(2.70192832106353,0.0795853421796018,4.84968068882004));
#7685=CARTESIAN_POINT('Ctrl Pts',(2.70944535996013,0.0872802053318244,4.84130181421633));
#7686=CARTESIAN_POINT('Ctrl Pts',(2.72625721055879,0.0974877239801237,4.82327328421564));
#7687=CARTESIAN_POINT('Ctrl Pts',(2.73556128485098,0.0999999999999996,4.81363205363199));
#7688=CARTESIAN_POINT('Ctrl Pts',(2.74444515022498,0.0999999999999996,4.80474818825798));
#7689=CARTESIAN_POINT('Ctrl Pts',(2.81837661840736,2.08166817117217E-17,
4.73725830020305));
#7690=CARTESIAN_POINT('Ctrl Pts',(2.81837661840736,-0.0125636537375776,
4.73725830020305));
#7691=CARTESIAN_POINT('Ctrl Pts',(2.8164323789192,-0.0259600177751461,4.7388669448893));
#7692=CARTESIAN_POINT('Ctrl Pts',(2.8086080061765,-0.0505959173616169,4.74547820056452));
#7693=CARTESIAN_POINT('Ctrl Pts',(2.80273676530252,-0.0618360346560354,
4.75048916218946));
#7694=CARTESIAN_POINT('Ctrl Pts',(2.78937765078703,-0.0795853421796016,
4.76223135909653));
#7695=CARTESIAN_POINT('Ctrl Pts',(2.78099877618333,-0.0872802053318249,
4.76974839799313));
#7696=CARTESIAN_POINT('Ctrl Pts',(2.76297024618264,-0.0974877239801236,
4.78656024859179));
#7697=CARTESIAN_POINT('Ctrl Pts',(2.75332901559899,-0.0999999999999996,
4.79586432288398));
#7698=CARTESIAN_POINT('Ctrl Pts',(2.73556128485098,-0.0999999999999996,
4.81363205363199));
#7699=CARTESIAN_POINT('Ctrl Pts',(2.72625721055879,-0.0974877239801236,
4.82327328421564));
#7700=CARTESIAN_POINT('Ctrl Pts',(2.70944535996013,-0.0872802053318249,
4.84130181421633));
#7701=CARTESIAN_POINT('Ctrl Pts',(2.70192832106353,-0.0795853421796018,
4.84968068882004));
#7702=CARTESIAN_POINT('Ctrl Pts',(2.69018612415646,-0.0618360346560355,
4.86303980333552));
#7703=CARTESIAN_POINT('Ctrl Pts',(2.68517516253152,-0.0505959173616165,
4.8689110442095));
#7704=CARTESIAN_POINT('Ctrl Pts',(2.6785639068563,-0.025960017775146,4.8767354169522));
#7705=CARTESIAN_POINT('Ctrl Pts',(2.67695526217005,-0.0125636537375776,
4.87867965644036));
#7706=CARTESIAN_POINT('Ctrl Pts',(2.67695526217005,-5.55111512312578E-17,
4.87867965644036));
#7707=CARTESIAN_POINT('',(2.7476659402887,-4.38851051975995E-18,4.66654762208439));
#7708=CARTESIAN_POINT('',(2.88908729652601,-1.22464679914735E-17,4.8079689783217));
#7709=CARTESIAN_POINT('',(2.60624458405139,-1.02865703380811E-16,4.8079689783217));
#7710=CARTESIAN_POINT('Ctrl Pts',(2.60624458405139,-3.81639164714898E-17,
4.8079689783217));
#7711=CARTESIAN_POINT('Ctrl Pts',(2.60624458405139,-0.0125652179652416,
4.8079689783217));
#7712=CARTESIAN_POINT('Ctrl Pts',(2.60783684799294,-0.0259622584309889,
4.80600749311067));
#7713=CARTESIAN_POINT('Ctrl Pts',(2.61438766218131,-0.0505977320073435,
4.79812203252307));
#7714=CARTESIAN_POINT('Ctrl Pts',(2.6193553527612,-0.0618368682969031,4.79220785299404));
#7715=CARTESIAN_POINT('Ctrl Pts',(2.63101522701612,-0.0795845181448063,
4.77876876013381));
#7716=CARTESIAN_POINT('Ctrl Pts',(2.63848820585999,-0.0872791387223183,
4.77034721873564));
#7717=CARTESIAN_POINT('Ctrl Pts',(2.65523838809476,-0.0974871089174108,
4.75225764285001));
#7718=CARTESIAN_POINT('Ctrl Pts',(2.66452586388438,-0.0999999999999996,
4.74259886406265));
#7719=CARTESIAN_POINT('Ctrl Pts',(2.68229582602965,-0.0999999999999996,
4.72482890191738));
#7720=CARTESIAN_POINT('Ctrl Pts',(2.69195460481701,-0.0974871089174108,
4.71554142612776));
#7721=CARTESIAN_POINT('Ctrl Pts',(2.71004418070264,-0.0872791387223183,
4.69879124389299));
#7722=CARTESIAN_POINT('Ctrl Pts',(2.71846572210081,-0.0795845181448063,
4.69131826504912));
#7723=CARTESIAN_POINT('Ctrl Pts',(2.73190481496104,-0.0618368682969031,
4.6796583907942));
#7724=CARTESIAN_POINT('Ctrl Pts',(2.73781899449007,-0.0505977320073435,
4.67469070021431));
#7725=CARTESIAN_POINT('Ctrl Pts',(2.74570445507767,-0.025962258430989,4.66813988602594));
#7726=CARTESIAN_POINT('Ctrl Pts',(2.7476659402887,-0.0125652179652417,4.66654762208439));
#7727=CARTESIAN_POINT('Ctrl Pts',(2.7476659402887,-7.97972798949331E-17,
4.66654762208439));
#7728=CARTESIAN_POINT('',(2.67341084495701,0.0999999999999997,4.73371388299002));
#7729=CARTESIAN_POINT('Ctrl Pts',(2.67341084495701,0.0999999999999997,4.73371388299002));
#7730=CARTESIAN_POINT('Ctrl Pts',(2.66452586388438,0.0999999999999997,4.74259886406265));
#7731=CARTESIAN_POINT('Ctrl Pts',(2.65523838809476,0.0974871089174108,4.75225764285001));
#7732=CARTESIAN_POINT('Ctrl Pts',(2.63848820585999,0.0872791387223183,4.77034721873564));
#7733=CARTESIAN_POINT('Ctrl Pts',(2.63101522701612,0.0795845181448063,4.77876876013381));
#7734=CARTESIAN_POINT('Ctrl Pts',(2.6193553527612,0.0618368682969031,4.79220785299404));
#7735=CARTESIAN_POINT('Ctrl Pts',(2.61438766218131,0.0505977320073435,4.79812203252307));
#7736=CARTESIAN_POINT('Ctrl Pts',(2.60783684799294,0.0259622584309889,4.80600749311067));
#7737=CARTESIAN_POINT('Ctrl Pts',(2.60624458405139,0.0125652179652416,4.8079689783217));
#7738=CARTESIAN_POINT('Ctrl Pts',(2.60624458405139,0.,4.8079689783217));
#7739=CARTESIAN_POINT('Ctrl Pts',(2.7476659402887,3.12250225675825E-17,
4.66654762208439));
#7740=CARTESIAN_POINT('Ctrl Pts',(2.7476659402887,0.0125652179652416,4.66654762208439));
#7741=CARTESIAN_POINT('Ctrl Pts',(2.74570445507767,0.0259622584309889,4.66813988602594));
#7742=CARTESIAN_POINT('Ctrl Pts',(2.73781899449007,0.0505977320073435,4.67469070021431));
#7743=CARTESIAN_POINT('Ctrl Pts',(2.73190481496104,0.0618368682969031,4.6796583907942));
#7744=CARTESIAN_POINT('Ctrl Pts',(2.71846572210081,0.0795845181448063,4.69131826504912));
#7745=CARTESIAN_POINT('Ctrl Pts',(2.71004418070264,0.0872791387223183,4.69879124389299));
#7746=CARTESIAN_POINT('Ctrl Pts',(2.69195460481701,0.0974871089174108,4.71554142612776));
#7747=CARTESIAN_POINT('Ctrl Pts',(2.68229582602965,0.0999999999999997,4.72482890191738));
#7748=CARTESIAN_POINT('Ctrl Pts',(2.67341084495701,0.0999999999999997,4.73371388299002));
#7749=CARTESIAN_POINT('Origin',(2.81837661840736,0.,4.87867965644036));
#7750=CARTESIAN_POINT('',(1.26628611700999,0.0999999999999997,3.32658915504299));
#7751=CARTESIAN_POINT('',(1.33345237791561,2.55038338414731E-18,3.2523340597113));
#7752=CARTESIAN_POINT('Ctrl Pts',(1.26628611700999,0.0999999999999996,3.32658915504299));
#7753=CARTESIAN_POINT('Ctrl Pts',(1.27517109808262,0.0999999999999996,3.31770417397035));
#7754=CARTESIAN_POINT('Ctrl Pts',(1.28445857387225,0.0974871089174108,3.30804539518299));
#7755=CARTESIAN_POINT('Ctrl Pts',(1.30120875610701,0.0872791387223183,3.28995581929736));
#7756=CARTESIAN_POINT('Ctrl Pts',(1.30868173495088,0.0795845181448063,3.28153427789919));
#7757=CARTESIAN_POINT('Ctrl Pts',(1.3203416092058,0.0618368682969031,3.26809518503896));
#7758=CARTESIAN_POINT('Ctrl Pts',(1.32530929978569,0.0505977320073435,3.26218100550993));
#7759=CARTESIAN_POINT('Ctrl Pts',(1.33186011397406,0.0259622584309889,3.25429554492233));
#7760=CARTESIAN_POINT('Ctrl Pts',(1.33345237791561,0.0125652179652415,3.2523340597113));
#7761=CARTESIAN_POINT('Ctrl Pts',(1.33345237791561,-5.20417042793042E-17,
3.2523340597113));
#7762=CARTESIAN_POINT('Ctrl Pts',(1.33345237791561,1.04083408558608E-17,
3.2523340597113));
#7763=CARTESIAN_POINT('Ctrl Pts',(1.33345237791561,-0.0125652179652416,
3.2523340597113));
#7764=CARTESIAN_POINT('Ctrl Pts',(1.33186011397406,-0.025962258430989,3.25429554492233));
#7765=CARTESIAN_POINT('Ctrl Pts',(1.32530929978569,-0.0505977320073435,
3.26218100550993));
#7766=CARTESIAN_POINT('Ctrl Pts',(1.3203416092058,-0.0618368682969031,3.26809518503896));
#7767=CARTESIAN_POINT('Ctrl Pts',(1.30868173495088,-0.0795845181448063,
3.28153427789919));
#7768=CARTESIAN_POINT('Ctrl Pts',(1.30120875610701,-0.0872791387223184,
3.28995581929736));
#7769=CARTESIAN_POINT('Ctrl Pts',(1.28445857387225,-0.0974871089174108,
3.30804539518299));
#7770=CARTESIAN_POINT('Ctrl Pts',(1.27517109808262,-0.0999999999999996,
3.31770417397035));
#7771=CARTESIAN_POINT('Ctrl Pts',(1.25740113593735,-0.0999999999999996,
3.33547413611562));
#7772=CARTESIAN_POINT('Ctrl Pts',(1.24774235714999,-0.0974871089174108,
3.34476161190525));
#7773=CARTESIAN_POINT('Ctrl Pts',(1.22965278126436,-0.0872791387223183,
3.36151179414001));
#7774=CARTESIAN_POINT('Ctrl Pts',(1.22123123986619,-0.0795845181448063,
3.36898477298388));
#7775=CARTESIAN_POINT('Ctrl Pts',(1.20779214700596,-0.0618368682969031,
3.3806446472388));
#7776=CARTESIAN_POINT('Ctrl Pts',(1.20187796747693,-0.0505977320073435,
3.38561233781869));
#7777=CARTESIAN_POINT('Ctrl Pts',(1.19399250688933,-0.0259622584309889,
3.39216315200706));
#7778=CARTESIAN_POINT('Ctrl Pts',(1.1920310216783,-0.0125652179652416,3.39375541594861));
#7779=CARTESIAN_POINT('Ctrl Pts',(1.1920310216783,0.0125652179652416,3.39375541594861));
#7780=CARTESIAN_POINT('Ctrl Pts',(1.19399250688933,0.0259622584309889,3.39216315200706));
#7781=CARTESIAN_POINT('Ctrl Pts',(1.20187796747693,0.0505977320073435,3.38561233781869));
#7782=CARTESIAN_POINT('Ctrl Pts',(1.20779214700596,0.0618368682969031,3.3806446472388));
#7783=CARTESIAN_POINT('Ctrl Pts',(1.22123123986619,0.0795845181448063,3.36898477298388));
#7784=CARTESIAN_POINT('Ctrl Pts',(1.22965278126436,0.0872791387223183,3.36151179414001));
#7785=CARTESIAN_POINT('Ctrl Pts',(1.24774235714999,0.0974871089174108,3.34476161190525));
#7786=CARTESIAN_POINT('Ctrl Pts',(1.25740113593735,0.0999999999999996,3.33547413611562));
#7787=CARTESIAN_POINT('Ctrl Pts',(1.26628611700999,0.0999999999999996,3.32658915504299));
#7788=CARTESIAN_POINT('',(1.26274169979695,-1.22464679914735E-17,3.18162338159264));
#7789=CARTESIAN_POINT('',(2.88908729652601,-1.22464679914735E-17,4.8079689783217));
#7790=CARTESIAN_POINT('',(1.19525181174202,0.0999999999999996,3.25555484977502));
#7791=CARTESIAN_POINT('Ctrl Pts',(1.19525181174202,0.0999999999999997,3.25555484977502));
#7792=CARTESIAN_POINT('Ctrl Pts',(1.18636794636801,0.0999999999999997,3.26443871514902));
#7793=CARTESIAN_POINT('Ctrl Pts',(1.17672671578436,0.0974877239801237,3.27374278944121));
#7794=CARTESIAN_POINT('Ctrl Pts',(1.15869818578367,0.0872802053318249,3.29055464003987));
#7795=CARTESIAN_POINT('Ctrl Pts',(1.15031931117997,0.0795853421796018,3.29807167893647));
#7796=CARTESIAN_POINT('Ctrl Pts',(1.13696019666448,0.0618360346560354,3.30981387584354));
#7797=CARTESIAN_POINT('Ctrl Pts',(1.1310889557905,0.0505959173616165,3.31482483746848));
#7798=CARTESIAN_POINT('Ctrl Pts',(1.1232645830478,0.025960017775146,3.3214360931437));
#7799=CARTESIAN_POINT('Ctrl Pts',(1.12132034355964,0.0125636537375776,3.32304473782995));
#7800=CARTESIAN_POINT('Ctrl Pts',(1.12132034355964,-0.0125636537375776,
3.32304473782995));
#7801=CARTESIAN_POINT('Ctrl Pts',(1.1232645830478,-0.0259600177751461,3.3214360931437));
#7802=CARTESIAN_POINT('Ctrl Pts',(1.1310889557905,-0.0505959173616165,3.31482483746848));
#7803=CARTESIAN_POINT('Ctrl Pts',(1.13696019666448,-0.0618360346560355,
3.30981387584354));
#7804=CARTESIAN_POINT('Ctrl Pts',(1.15031931117997,-0.0795853421796018,
3.29807167893647));
#7805=CARTESIAN_POINT('Ctrl Pts',(1.15869818578367,-0.087280205331825,3.29055464003987));
#7806=CARTESIAN_POINT('Ctrl Pts',(1.17672671578436,-0.0974877239801237,
3.27374278944121));
#7807=CARTESIAN_POINT('Ctrl Pts',(1.18636794636801,-0.0999999999999996,
3.26443871514902));
#7808=CARTESIAN_POINT('Ctrl Pts',(1.20413567711602,-0.0999999999999996,
3.24667098440101));
#7809=CARTESIAN_POINT('Ctrl Pts',(1.21343975140821,-0.0974877239801237,
3.23702975381736));
#7810=CARTESIAN_POINT('Ctrl Pts',(1.23025160200687,-0.0872802053318249,
3.21900122381667));
#7811=CARTESIAN_POINT('Ctrl Pts',(1.23776864090347,-0.0795853421796016,
3.21062234921297));
#7812=CARTESIAN_POINT('Ctrl Pts',(1.24951083781054,-0.0618360346560355,
3.19726323469748));
#7813=CARTESIAN_POINT('Ctrl Pts',(1.25452179943548,-0.0505959173616169,
3.1913919938235));
#7814=CARTESIAN_POINT('Ctrl Pts',(1.2611330551107,-0.0259600177751461,3.1835676210808));
#7815=CARTESIAN_POINT('Ctrl Pts',(1.26274169979695,-0.0125636537375777,
3.18162338159264));
#7816=CARTESIAN_POINT('Ctrl Pts',(1.26274169979695,1.73472347597681E-17,
3.18162338159264));
#7817=CARTESIAN_POINT('Ctrl Pts',(1.26274169979695,1.38777878078145E-17,
3.18162338159264));
#7818=CARTESIAN_POINT('Ctrl Pts',(1.26274169979695,0.0125636537375777,3.18162338159264));
#7819=CARTESIAN_POINT('Ctrl Pts',(1.2611330551107,0.0259600177751461,3.1835676210808));
#7820=CARTESIAN_POINT('Ctrl Pts',(1.25452179943548,0.0505959173616169,3.1913919938235));
#7821=CARTESIAN_POINT('Ctrl Pts',(1.24951083781054,0.0618360346560355,3.19726323469748));
#7822=CARTESIAN_POINT('Ctrl Pts',(1.23776864090347,0.0795853421796016,3.21062234921297));
#7823=CARTESIAN_POINT('Ctrl Pts',(1.23025160200687,0.087280205331825,3.21900122381667));
#7824=CARTESIAN_POINT('Ctrl Pts',(1.21343975140821,0.0974877239801238,3.23702975381736));
#7825=CARTESIAN_POINT('Ctrl Pts',(1.20413567711602,0.0999999999999996,3.24667098440101));
#7826=CARTESIAN_POINT('Ctrl Pts',(1.19525181174202,0.0999999999999996,3.25555484977502));
#7827=CARTESIAN_POINT('Origin',(2.25269119345812,0.,5.4443650813896));
#7828=CARTESIAN_POINT('',(2.17875972527575,0.1,5.37043361320722));
#7829=CARTESIAN_POINT('',(2.25269119345812,-1.22464679914735E-17,5.30294372515229));
#7830=CARTESIAN_POINT('Ctrl Pts',(2.17875972527575,0.1,5.37043361320722));
#7831=CARTESIAN_POINT('Ctrl Pts',(2.18764359064975,0.1,5.36154974783322));
#7832=CARTESIAN_POINT('Ctrl Pts',(2.1972848212334,0.0974877239801244,5.35224567354103));
#7833=CARTESIAN_POINT('Ctrl Pts',(2.21531335123409,0.0872802053318256,5.33543382294237));
#7834=CARTESIAN_POINT('Ctrl Pts',(2.2236922258378,0.0795853421796021,5.32791678404577));
#7835=CARTESIAN_POINT('Ctrl Pts',(2.23705134035328,0.0618360346560359,5.3161745871387));
#7836=CARTESIAN_POINT('Ctrl Pts',(2.24292258122726,0.0505959173616174,5.31116362551376));
#7837=CARTESIAN_POINT('Ctrl Pts',(2.25074695396996,0.0259600177751464,5.30455236983854));
#7838=CARTESIAN_POINT('Ctrl Pts',(2.25269119345812,0.0125636537375777,5.30294372515229));
#7839=CARTESIAN_POINT('Ctrl Pts',(2.25269119345812,-1.73472347597681E-17,
5.30294372515229));
#7840=CARTESIAN_POINT('',(2.11126983722081,-7.42944678570117E-17,5.4443650813896));
#7841=CARTESIAN_POINT('Ctrl Pts',(2.11126983722081,-2.08166817117217E-17,
5.4443650813896));
#7842=CARTESIAN_POINT('Ctrl Pts',(2.11126983722081,0.0125636537375776,5.4443650813896));
#7843=CARTESIAN_POINT('Ctrl Pts',(2.11287848190706,0.025960017775146,5.44242084190144));
#7844=CARTESIAN_POINT('Ctrl Pts',(2.11948973758228,0.050595917361617,5.43459646915874));
#7845=CARTESIAN_POINT('Ctrl Pts',(2.12450069920722,0.0618360346560357,5.42872522828476));
#7846=CARTESIAN_POINT('Ctrl Pts',(2.13624289611429,0.0795853421796022,5.41536611376927));
#7847=CARTESIAN_POINT('Ctrl Pts',(2.14375993501089,0.0872802053318249,5.40698723916557));
#7848=CARTESIAN_POINT('Ctrl Pts',(2.16057178560955,0.097487723980124,5.38895870916488));
#7849=CARTESIAN_POINT('Ctrl Pts',(2.16987585990174,0.1,5.37931747858123));
#7850=CARTESIAN_POINT('Ctrl Pts',(2.17875972527575,0.1,5.37043361320722));
#7851=CARTESIAN_POINT('Ctrl Pts',(2.25269119345812,3.81639164714898E-17,
5.30294372515229));
#7852=CARTESIAN_POINT('Ctrl Pts',(2.25269119345812,-0.0125636537375776,
5.30294372515229));
#7853=CARTESIAN_POINT('Ctrl Pts',(2.25074695396996,-0.0259600177751464,
5.30455236983854));
#7854=CARTESIAN_POINT('Ctrl Pts',(2.24292258122726,-0.0505959173616173,
5.31116362551376));
#7855=CARTESIAN_POINT('Ctrl Pts',(2.23705134035328,-0.0618360346560359,
5.3161745871387));
#7856=CARTESIAN_POINT('Ctrl Pts',(2.2236922258378,-0.0795853421796021,5.32791678404577));
#7857=CARTESIAN_POINT('Ctrl Pts',(2.21531335123409,-0.0872802053318256,
5.33543382294237));
#7858=CARTESIAN_POINT('Ctrl Pts',(2.1972848212334,-0.0974877239801244,5.35224567354103));
#7859=CARTESIAN_POINT('Ctrl Pts',(2.18764359064975,-0.1,5.36154974783322));
#7860=CARTESIAN_POINT('Ctrl Pts',(2.16987585990174,-0.1,5.37931747858123));
#7861=CARTESIAN_POINT('Ctrl Pts',(2.16057178560955,-0.0974877239801244,
5.38895870916487));
#7862=CARTESIAN_POINT('Ctrl Pts',(2.14375993501089,-0.0872802053318256,
5.40698723916557));
#7863=CARTESIAN_POINT('Ctrl Pts',(2.13624289611429,-0.0795853421796021,
5.41536611376927));
#7864=CARTESIAN_POINT('Ctrl Pts',(2.12450069920722,-0.0618360346560358,
5.42872522828476));
#7865=CARTESIAN_POINT('Ctrl Pts',(2.11948973758228,-0.0505959173616171,
5.43459646915874));
#7866=CARTESIAN_POINT('Ctrl Pts',(2.11287848190706,-0.0259600177751462,
5.44242084190144));
#7867=CARTESIAN_POINT('Ctrl Pts',(2.11126983722081,-0.0125636537375778,
5.4443650813896));
#7868=CARTESIAN_POINT('Ctrl Pts',(2.11126983722081,-6.93889390390723E-17,
5.4443650813896));
#7869=CARTESIAN_POINT('',(2.18198051533946,-1.13274044236672E-17,5.23223304703363));
#7870=CARTESIAN_POINT('',(2.32340187157677,-1.22464679914735E-17,5.37365440327094));
#7871=CARTESIAN_POINT('',(2.04055915910216,-2.65378704378315E-17,5.37365440327094));
#7872=CARTESIAN_POINT('Ctrl Pts',(2.04055915910216,6.93889390390723E-18,
5.37365440327094));
#7873=CARTESIAN_POINT('Ctrl Pts',(2.04055915910216,-0.0125652179652417,
5.37365440327094));
#7874=CARTESIAN_POINT('Ctrl Pts',(2.0421514230437,-0.0259622584309895,5.37169291805991));
#7875=CARTESIAN_POINT('Ctrl Pts',(2.04870223723207,-0.0505977320073441,
5.36380745747231));
#7876=CARTESIAN_POINT('Ctrl Pts',(2.05366992781196,-0.0618368682969035,
5.35789327794327));
#7877=CARTESIAN_POINT('Ctrl Pts',(2.06532980206688,-0.0795845181448067,
5.34445418508304));
#7878=CARTESIAN_POINT('Ctrl Pts',(2.07280278091075,-0.0872791387223187,
5.33603264368488));
#7879=CARTESIAN_POINT('Ctrl Pts',(2.08955296314552,-0.0974871089174111,
5.31794306779925));
#7880=CARTESIAN_POINT('Ctrl Pts',(2.09884043893515,-0.1,5.30828428901188));
#7881=CARTESIAN_POINT('Ctrl Pts',(2.11661040108041,-0.1,5.29051432686662));
#7882=CARTESIAN_POINT('Ctrl Pts',(2.12626917986777,-0.0974871089174109,
5.28122685107699));
#7883=CARTESIAN_POINT('Ctrl Pts',(2.1443587557534,-0.0872791387223181,5.26447666884223));
#7884=CARTESIAN_POINT('Ctrl Pts',(2.15278029715157,-0.0795845181448065,
5.25700368999836));
#7885=CARTESIAN_POINT('Ctrl Pts',(2.1662193900118,-0.0618368682969033,5.24534381574343));
#7886=CARTESIAN_POINT('Ctrl Pts',(2.17213356954083,-0.0505977320073437,
5.24037612516355));
#7887=CARTESIAN_POINT('Ctrl Pts',(2.18001903012844,-0.0259622584309892,
5.23382531097518));
#7888=CARTESIAN_POINT('Ctrl Pts',(2.18198051533946,-0.0125652179652416,
5.23223304703363));
#7889=CARTESIAN_POINT('Ctrl Pts',(2.18198051533946,-2.77555756156289E-17,
5.23223304703363));
#7890=CARTESIAN_POINT('',(2.10772542000778,0.1,5.29939930793925));
#7891=CARTESIAN_POINT('Ctrl Pts',(2.10772542000778,0.1,5.29939930793925));
#7892=CARTESIAN_POINT('Ctrl Pts',(2.09884043893515,0.1,5.30828428901188));
#7893=CARTESIAN_POINT('Ctrl Pts',(2.08955296314552,0.0974871089174111,5.31794306779925));
#7894=CARTESIAN_POINT('Ctrl Pts',(2.07280278091075,0.0872791387223187,5.33603264368488));
#7895=CARTESIAN_POINT('Ctrl Pts',(2.06532980206688,0.0795845181448067,5.34445418508304));
#7896=CARTESIAN_POINT('Ctrl Pts',(2.05366992781196,0.0618368682969035,5.35789327794327));
#7897=CARTESIAN_POINT('Ctrl Pts',(2.04870223723207,0.0505977320073439,5.36380745747231));
#7898=CARTESIAN_POINT('Ctrl Pts',(2.0421514230437,0.0259622584309892,5.37169291805991));
#7899=CARTESIAN_POINT('Ctrl Pts',(2.04055915910215,0.0125652179652417,5.37365440327094));
#7900=CARTESIAN_POINT('Ctrl Pts',(2.04055915910215,-3.46944695195361E-18,
5.37365440327094));
#7901=CARTESIAN_POINT('Ctrl Pts',(2.18198051533946,0.,5.23223304703363));
#7902=CARTESIAN_POINT('Ctrl Pts',(2.18198051533946,0.0125652179652416,5.23223304703363));
#7903=CARTESIAN_POINT('Ctrl Pts',(2.18001903012844,0.0259622584309892,5.23382531097518));
#7904=CARTESIAN_POINT('Ctrl Pts',(2.17213356954083,0.0505977320073437,5.24037612516355));
#7905=CARTESIAN_POINT('Ctrl Pts',(2.1662193900118,0.0618368682969032,5.24534381574343));
#7906=CARTESIAN_POINT('Ctrl Pts',(2.15278029715157,0.0795845181448064,5.25700368999836));
#7907=CARTESIAN_POINT('Ctrl Pts',(2.1443587557534,0.0872791387223183,5.26447666884223));
#7908=CARTESIAN_POINT('Ctrl Pts',(2.12626917986777,0.097487108917411,5.28122685107699));
#7909=CARTESIAN_POINT('Ctrl Pts',(2.11661040108041,0.1,5.29051432686662));
#7910=CARTESIAN_POINT('Ctrl Pts',(2.10772542000778,0.1,5.29939930793925));
#7911=CARTESIAN_POINT('Origin',(2.25269119345812,0.,5.4443650813896));
#7912=CARTESIAN_POINT('',(0.700600692060748,0.1,3.89227457999222));
#7913=CARTESIAN_POINT('',(0.76776695296637,-3.90829800392961E-17,3.81801948466054));
#7914=CARTESIAN_POINT('Ctrl Pts',(0.700600692060748,0.1,3.89227457999222));
#7915=CARTESIAN_POINT('Ctrl Pts',(0.709485673133379,0.1,3.88338959891959));
#7916=CARTESIAN_POINT('Ctrl Pts',(0.718773148923008,0.097487108917411,3.87373082013223));
#7917=CARTESIAN_POINT('Ctrl Pts',(0.735523331157776,0.0872791387223179,
3.8556412442466));
#7918=CARTESIAN_POINT('Ctrl Pts',(0.742996310001643,0.0795845181448064,
3.84721970284843));
#7919=CARTESIAN_POINT('Ctrl Pts',(0.754656184256567,0.0618368682969032,
3.8337806099882));
#7920=CARTESIAN_POINT('Ctrl Pts',(0.75962387483645,0.0505977320073437,3.82786643045917));
#7921=CARTESIAN_POINT('Ctrl Pts',(0.766174689024822,0.0259622584309892,
3.81998096987156));
#7922=CARTESIAN_POINT('Ctrl Pts',(0.76776695296637,0.0125652179652416,3.81801948466054));
#7923=CARTESIAN_POINT('Ctrl Pts',(0.76776695296637,-2.42861286636753E-17,
3.81801948466054));
#7924=CARTESIAN_POINT('Ctrl Pts',(0.76776695296637,-6.24500451351651E-17,
3.81801948466054));
#7925=CARTESIAN_POINT('Ctrl Pts',(0.76776695296637,-0.0125652179652416,
3.81801948466054));
#7926=CARTESIAN_POINT('Ctrl Pts',(0.766174689024822,-0.0259622584309892,
3.81998096987156));
#7927=CARTESIAN_POINT('Ctrl Pts',(0.75962387483645,-0.0505977320073437,
3.82786643045917));
#7928=CARTESIAN_POINT('Ctrl Pts',(0.754656184256567,-0.0618368682969033,
3.8337806099882));
#7929=CARTESIAN_POINT('Ctrl Pts',(0.742996310001643,-0.0795845181448065,
3.84721970284843));
#7930=CARTESIAN_POINT('Ctrl Pts',(0.735523331157776,-0.0872791387223179,
3.8556412442466));
#7931=CARTESIAN_POINT('Ctrl Pts',(0.718773148923008,-0.0974871089174109,
3.87373082013223));
#7932=CARTESIAN_POINT('Ctrl Pts',(0.709485673133379,-0.1,3.88338959891959));
#7933=CARTESIAN_POINT('Ctrl Pts',(0.691715710988117,-0.1,3.90115956106485));
#7934=CARTESIAN_POINT('Ctrl Pts',(0.68205693220075,-0.0974871089174111,
3.91044703685448));
#7935=CARTESIAN_POINT('Ctrl Pts',(0.663967356315122,-0.0872791387223187,
3.92719721908925));
#7936=CARTESIAN_POINT('Ctrl Pts',(0.655545814916956,-0.0795845181448067,
3.93467019793312));
#7937=CARTESIAN_POINT('Ctrl Pts',(0.642106722056726,-0.0618368682969035,
3.94633007218804));
#7938=CARTESIAN_POINT('Ctrl Pts',(0.63619254252769,-0.0505977320073439,
3.95129776276793));
#7939=CARTESIAN_POINT('Ctrl Pts',(0.628307081940087,-0.0259622584309892,
3.9578485769563));
#7940=CARTESIAN_POINT('Ctrl Pts',(0.62634559672906,-0.0125652179652417,
3.95944084089785));
#7941=CARTESIAN_POINT('Ctrl Pts',(0.62634559672906,0.0125652179652417,3.95944084089785));
#7942=CARTESIAN_POINT('Ctrl Pts',(0.628307081940087,0.0259622584309892,
3.9578485769563));
#7943=CARTESIAN_POINT('Ctrl Pts',(0.63619254252769,0.0505977320073439,3.95129776276793));
#7944=CARTESIAN_POINT('Ctrl Pts',(0.642106722056726,0.0618368682969035,
3.94633007218804));
#7945=CARTESIAN_POINT('Ctrl Pts',(0.655545814916956,0.0795845181448067,
3.93467019793312));
#7946=CARTESIAN_POINT('Ctrl Pts',(0.663967356315122,0.0872791387223187,
3.92719721908925));
#7947=CARTESIAN_POINT('Ctrl Pts',(0.68205693220075,0.0974871089174111,3.91044703685448));
#7948=CARTESIAN_POINT('Ctrl Pts',(0.691715710988117,0.1,3.90115956106486));
#7949=CARTESIAN_POINT('Ctrl Pts',(0.700600692060748,0.1,3.89227457999222));
#7950=CARTESIAN_POINT('',(0.697056274847714,-1.22464679914735E-17,3.74730880654188));
#7951=CARTESIAN_POINT('',(2.32340187157677,-1.22464679914735E-17,5.37365440327094));
#7952=CARTESIAN_POINT('',(0.629566386792779,0.1,3.82124027472426));
#7953=CARTESIAN_POINT('Ctrl Pts',(0.629566386792779,0.1,3.82124027472426));
#7954=CARTESIAN_POINT('Ctrl Pts',(0.620682521418773,0.1,3.83012414009826));
#7955=CARTESIAN_POINT('Ctrl Pts',(0.611041290835125,0.0974877239801243,
3.83942821439045));
#7956=CARTESIAN_POINT('Ctrl Pts',(0.593012760834431,0.0872802053318254,
3.85624006498911));
#7957=CARTESIAN_POINT('Ctrl Pts',(0.584633886230728,0.0795853421796021,
3.86375710388571));
#7958=CARTESIAN_POINT('Ctrl Pts',(0.571274771715239,0.0618360346560357,
3.87549930079278));
#7959=CARTESIAN_POINT('Ctrl Pts',(0.565403530841261,0.050595917361617,3.88051026241772));
#7960=CARTESIAN_POINT('Ctrl Pts',(0.557579158098564,0.025960017775146,3.88712151809294));
#7961=CARTESIAN_POINT('Ctrl Pts',(0.555634918610405,0.0125636537375776,
3.88873016277919));
#7962=CARTESIAN_POINT('Ctrl Pts',(0.555634918610405,-0.0125636537375777,
3.88873016277919));
#7963=CARTESIAN_POINT('Ctrl Pts',(0.557579158098565,-0.0259600177751462,
3.88712151809294));
#7964=CARTESIAN_POINT('Ctrl Pts',(0.565403530841262,-0.0505959173616171,
3.88051026241772));
#7965=CARTESIAN_POINT('Ctrl Pts',(0.57127477171524,-0.0618360346560357,
3.87549930079278));
#7966=CARTESIAN_POINT('Ctrl Pts',(0.584633886230728,-0.0795853421796021,
3.86375710388571));
#7967=CARTESIAN_POINT('Ctrl Pts',(0.593012760834432,-0.0872802053318256,
3.85624006498911));
#7968=CARTESIAN_POINT('Ctrl Pts',(0.611041290835125,-0.0974877239801244,
3.83942821439045));
#7969=CARTESIAN_POINT('Ctrl Pts',(0.620682521418773,-0.1,3.83012414009826));
#7970=CARTESIAN_POINT('Ctrl Pts',(0.638450252166784,-0.1,3.81235640935025));
#7971=CARTESIAN_POINT('Ctrl Pts',(0.647754326458969,-0.0974877239801244,
3.8027151787666));
#7972=CARTESIAN_POINT('Ctrl Pts',(0.664566177057634,-0.0872802053318256,
3.78468664876591));
#7973=CARTESIAN_POINT('Ctrl Pts',(0.672083215954231,-0.0795853421796021,
3.7763077741622));
#7974=CARTESIAN_POINT('Ctrl Pts',(0.683825412861301,-0.0618360346560359,
3.76294865964672));
#7975=CARTESIAN_POINT('Ctrl Pts',(0.688836374486244,-0.050595917361617,
3.75707741877274));
#7976=CARTESIAN_POINT('Ctrl Pts',(0.695447630161466,-0.0259600177751463,
3.74925304603004));
#7977=CARTESIAN_POINT('Ctrl Pts',(0.697056274847715,-0.0125636537375777,
3.74730880654188));
#7978=CARTESIAN_POINT('Ctrl Pts',(0.697056274847715,-2.08166817117217E-17,
3.74730880654188));
#7979=CARTESIAN_POINT('Ctrl Pts',(0.697056274847715,1.04083408558608E-17,
3.74730880654188));
#7980=CARTESIAN_POINT('Ctrl Pts',(0.697056274847715,0.0125636537375777,
3.74730880654188));
#7981=CARTESIAN_POINT('Ctrl Pts',(0.695447630161466,0.0259600177751463,
3.74925304603004));
#7982=CARTESIAN_POINT('Ctrl Pts',(0.688836374486244,0.050595917361617,3.75707741877274));
#7983=CARTESIAN_POINT('Ctrl Pts',(0.683825412861301,0.0618360346560359,
3.76294865964672));
#7984=CARTESIAN_POINT('Ctrl Pts',(0.672083215954231,0.0795853421796021,
3.7763077741622));
#7985=CARTESIAN_POINT('Ctrl Pts',(0.664566177057633,0.087280205331826,3.78468664876591));
#7986=CARTESIAN_POINT('Ctrl Pts',(0.647754326458969,0.0974877239801246,
3.8027151787666));
#7987=CARTESIAN_POINT('Ctrl Pts',(0.638450252166784,0.1,3.81235640935025));
#7988=CARTESIAN_POINT('Ctrl Pts',(0.629566386792779,0.1,3.82124027472426));
#7989=CARTESIAN_POINT('Origin',(1.68700576850888,0.,6.01005050633883));
#7990=CARTESIAN_POINT('',(1.61307430032651,0.1,5.93611903815646));
#7991=CARTESIAN_POINT('',(1.68700576850888,-1.22464679914735E-17,5.86862915010152));
#7992=CARTESIAN_POINT('Ctrl Pts',(1.61307430032651,0.1,5.93611903815646));
#7993=CARTESIAN_POINT('Ctrl Pts',(1.62195816570051,0.1,5.92723517278246));
#7994=CARTESIAN_POINT('Ctrl Pts',(1.63159939628416,0.0974877239801244,5.91793109849027));
#7995=CARTESIAN_POINT('Ctrl Pts',(1.64962792628485,0.0872802053318256,5.90111924789161));
#7996=CARTESIAN_POINT('Ctrl Pts',(1.65800680088856,0.0795853421796021,5.89360220899501));
#7997=CARTESIAN_POINT('Ctrl Pts',(1.67136591540405,0.0618360346560357,5.88186001208794));
#7998=CARTESIAN_POINT('Ctrl Pts',(1.67723715627803,0.050595917361617,5.87684905046299));
#7999=CARTESIAN_POINT('Ctrl Pts',(1.68506152902072,0.0259600177751461,5.87023779478777));
#8000=CARTESIAN_POINT('Ctrl Pts',(1.68700576850888,0.0125636537375777,5.86862915010152));
#8001=CARTESIAN_POINT('Ctrl Pts',(1.68700576850888,1.30104260698261E-17,
5.86862915010152));
#8002=CARTESIAN_POINT('',(1.54558441227157,-8.29680852368957E-17,6.01005050633883));
#8003=CARTESIAN_POINT('Ctrl Pts',(1.54558441227157,-4.5102810375397E-17,
6.01005050633883));
#8004=CARTESIAN_POINT('Ctrl Pts',(1.54558441227157,0.0125636537375776,6.01005050633883));
#8005=CARTESIAN_POINT('Ctrl Pts',(1.54719305695782,0.025960017775146,6.00810626685067));
#8006=CARTESIAN_POINT('Ctrl Pts',(1.55380431263304,0.050595917361617,6.00028189410798));
#8007=CARTESIAN_POINT('Ctrl Pts',(1.55881527425799,0.0618360346560357,5.994410653234));
#8008=CARTESIAN_POINT('Ctrl Pts',(1.57055747116505,0.0795853421796021,5.98105153871851));
#8009=CARTESIAN_POINT('Ctrl Pts',(1.57807451006165,0.0872802053318254,5.97267266411481));
#8010=CARTESIAN_POINT('Ctrl Pts',(1.59488636066032,0.0974877239801243,5.95464413411411));
#8011=CARTESIAN_POINT('Ctrl Pts',(1.6041904349525,0.1,5.94500290353047));
#8012=CARTESIAN_POINT('Ctrl Pts',(1.61307430032651,0.1,5.93611903815646));
#8013=CARTESIAN_POINT('Ctrl Pts',(1.68700576850888,-2.42861286636753E-17,
5.86862915010152));
#8014=CARTESIAN_POINT('Ctrl Pts',(1.68700576850888,-0.0125636537375777,
5.86862915010152));
#8015=CARTESIAN_POINT('Ctrl Pts',(1.68506152902072,-0.025960017775146,5.87023779478777));
#8016=CARTESIAN_POINT('Ctrl Pts',(1.67723715627803,-0.050595917361617,5.87684905046299));
#8017=CARTESIAN_POINT('Ctrl Pts',(1.67136591540405,-0.0618360346560357,
5.88186001208794));
#8018=CARTESIAN_POINT('Ctrl Pts',(1.65800680088856,-0.0795853421796022,
5.89360220899501));
#8019=CARTESIAN_POINT('Ctrl Pts',(1.64962792628485,-0.0872802053318254,
5.9011192478916));
#8020=CARTESIAN_POINT('Ctrl Pts',(1.63159939628416,-0.0974877239801242,
5.91793109849027));
#8021=CARTESIAN_POINT('Ctrl Pts',(1.62195816570051,-0.1,5.92723517278245));
#8022=CARTESIAN_POINT('Ctrl Pts',(1.6041904349525,-0.1,5.94500290353047));
#8023=CARTESIAN_POINT('Ctrl Pts',(1.59488636066032,-0.0974877239801244,
5.95464413411411));
#8024=CARTESIAN_POINT('Ctrl Pts',(1.57807451006165,-0.0872802053318256,
5.97267266411481));
#8025=CARTESIAN_POINT('Ctrl Pts',(1.57055747116505,-0.0795853421796021,
5.98105153871851));
#8026=CARTESIAN_POINT('Ctrl Pts',(1.55881527425799,-0.0618360346560358,
5.994410653234));
#8027=CARTESIAN_POINT('Ctrl Pts',(1.55380431263304,-0.050595917361617,6.00028189410798));
#8028=CARTESIAN_POINT('Ctrl Pts',(1.54719305695782,-0.0259600177751461,
6.00810626685067));
#8029=CARTESIAN_POINT('Ctrl Pts',(1.54558441227157,-0.0125636537375777,
6.01005050633883));
#8030=CARTESIAN_POINT('Ctrl Pts',(1.54558441227157,-3.81639164714898E-17,
6.01005050633883));
#8031=CARTESIAN_POINT('',(1.61629509039023,-1.47968513756208E-17,5.79791847198287));
#8032=CARTESIAN_POINT('',(1.75771644662754,-1.22464679914735E-17,5.93933982822018));
#8033=CARTESIAN_POINT('',(1.47487373415292,-5.08239991015068E-17,5.93933982822018));
#8034=CARTESIAN_POINT('Ctrl Pts',(1.47487373415292,1.73472347597681E-17,
5.93933982822018));
#8035=CARTESIAN_POINT('Ctrl Pts',(1.47487373415292,-0.0125652179652416,
5.93933982822018));
#8036=CARTESIAN_POINT('Ctrl Pts',(1.47646599809446,-0.0259622584309893,
5.93737834300915));
#8037=CARTESIAN_POINT('Ctrl Pts',(1.48301681228284,-0.0505977320073439,
5.92949288242155));
#8038=CARTESIAN_POINT('Ctrl Pts',(1.48798450286272,-0.0618368682969034,
5.92357870289251));
#8039=CARTESIAN_POINT('Ctrl Pts',(1.49964437711764,-0.0795845181448066,
5.91013961003228));
#8040=CARTESIAN_POINT('Ctrl Pts',(1.50711735596151,-0.0872791387223186,
5.90171806863412));
#8041=CARTESIAN_POINT('Ctrl Pts',(1.52386753819628,-0.0974871089174113,
5.88362849274849));
#8042=CARTESIAN_POINT('Ctrl Pts',(1.53315501398591,-0.1,5.87396971396112));
#8043=CARTESIAN_POINT('Ctrl Pts',(1.55092497613117,-0.1,5.85619975181586));
#8044=CARTESIAN_POINT('Ctrl Pts',(1.56058375491854,-0.0974871089174112,
5.84691227602623));
#8045=CARTESIAN_POINT('Ctrl Pts',(1.57867333080416,-0.0872791387223186,
5.83016209379146));
#8046=CARTESIAN_POINT('Ctrl Pts',(1.58709487220233,-0.0795845181448066,
5.8226891149476));
#8047=CARTESIAN_POINT('Ctrl Pts',(1.60053396506256,-0.0618368682969034,
5.81102924069267));
#8048=CARTESIAN_POINT('Ctrl Pts',(1.6064481445916,-0.0505977320073438,5.80606155011279));
#8049=CARTESIAN_POINT('Ctrl Pts',(1.6143336051792,-0.0259622584309891,5.79951073592442));
#8050=CARTESIAN_POINT('Ctrl Pts',(1.61629509039023,-0.0125652179652417,
5.79791847198287));
#8051=CARTESIAN_POINT('Ctrl Pts',(1.61629509039023,-3.81639164714898E-17,
5.79791847198287));
#8052=CARTESIAN_POINT('',(1.54203999505854,0.1,5.86508473288849));
#8053=CARTESIAN_POINT('Ctrl Pts',(1.54203999505854,0.1,5.86508473288849));
#8054=CARTESIAN_POINT('Ctrl Pts',(1.53315501398591,0.1,5.87396971396112));
#8055=CARTESIAN_POINT('Ctrl Pts',(1.52386753819628,0.0974871089174112,5.88362849274849));
#8056=CARTESIAN_POINT('Ctrl Pts',(1.50711735596151,0.0872791387223186,5.90171806863412));
#8057=CARTESIAN_POINT('Ctrl Pts',(1.49964437711764,0.0795845181448066,5.91013961003228));
#8058=CARTESIAN_POINT('Ctrl Pts',(1.48798450286272,0.0618368682969034,5.92357870289251));
#8059=CARTESIAN_POINT('Ctrl Pts',(1.48301681228284,0.0505977320073438,5.92949288242155));
#8060=CARTESIAN_POINT('Ctrl Pts',(1.47646599809446,0.0259622584309891,5.93737834300915));
#8061=CARTESIAN_POINT('Ctrl Pts',(1.47487373415292,0.0125652179652416,5.93933982822018));
#8062=CARTESIAN_POINT('Ctrl Pts',(1.47487373415292,-9.71445146547012E-17,
5.93933982822018));
#8063=CARTESIAN_POINT('Ctrl Pts',(1.61629509039023,-1.73472347597681E-17,
5.79791847198287));
#8064=CARTESIAN_POINT('Ctrl Pts',(1.61629509039023,0.0125652179652416,5.79791847198287));
#8065=CARTESIAN_POINT('Ctrl Pts',(1.6143336051792,0.0259622584309893,5.79951073592442));
#8066=CARTESIAN_POINT('Ctrl Pts',(1.6064481445916,0.0505977320073438,5.80606155011279));
#8067=CARTESIAN_POINT('Ctrl Pts',(1.60053396506256,0.0618368682969034,5.81102924069267));
#8068=CARTESIAN_POINT('Ctrl Pts',(1.58709487220233,0.0795845181448067,5.8226891149476));
#8069=CARTESIAN_POINT('Ctrl Pts',(1.57867333080416,0.0872791387223186,5.83016209379146));
#8070=CARTESIAN_POINT('Ctrl Pts',(1.56058375491854,0.097487108917411,5.84691227602623));
#8071=CARTESIAN_POINT('Ctrl Pts',(1.55092497613117,0.1,5.85619975181586));
#8072=CARTESIAN_POINT('Ctrl Pts',(1.54203999505854,0.1,5.86508473288849));
#8073=CARTESIAN_POINT('Origin',(1.68700576850888,0.,6.01005050633883));
#8074=CARTESIAN_POINT('',(0.13491526711151,0.1,4.45796000494146));
#8075=CARTESIAN_POINT('',(0.202081528017132,-2.86746391834353E-17,4.38370490960977));
#8076=CARTESIAN_POINT('Ctrl Pts',(0.13491526711151,0.1,4.45796000494146));
#8077=CARTESIAN_POINT('Ctrl Pts',(0.143800248184141,0.1,4.44907502386883));
#8078=CARTESIAN_POINT('Ctrl Pts',(0.15308772397377,0.097487108917411,4.43941624508146));
#8079=CARTESIAN_POINT('Ctrl Pts',(0.169837906208537,0.0872791387223186,
4.42132666919584));
#8080=CARTESIAN_POINT('Ctrl Pts',(0.177310885052405,0.0795845181448067,
4.41290512779767));
#8081=CARTESIAN_POINT('Ctrl Pts',(0.188970759307329,0.0618368682969034,
4.39946603493744));
#8082=CARTESIAN_POINT('Ctrl Pts',(0.193938449887212,0.0505977320073438,
4.3935518554084));
#8083=CARTESIAN_POINT('Ctrl Pts',(0.200489264075584,0.0259622584309893,
4.3856663948208));
#8084=CARTESIAN_POINT('Ctrl Pts',(0.202081528017132,0.0125652179652416,
4.38370490960977));
#8085=CARTESIAN_POINT('Ctrl Pts',(0.202081528017132,-3.81639164714898E-17,
4.38370490960977));
#8086=CARTESIAN_POINT('Ctrl Pts',(0.202081528017132,-4.5102810375397E-17,
4.38370490960977));
#8087=CARTESIAN_POINT('Ctrl Pts',(0.202081528017132,-0.0125652179652417,
4.38370490960977));
#8088=CARTESIAN_POINT('Ctrl Pts',(0.200489264075584,-0.0259622584309891,
4.3856663948208));
#8089=CARTESIAN_POINT('Ctrl Pts',(0.193938449887212,-0.0505977320073438,
4.3935518554084));
#8090=CARTESIAN_POINT('Ctrl Pts',(0.188970759307328,-0.0618368682969034,
4.39946603493744));
#8091=CARTESIAN_POINT('Ctrl Pts',(0.177310885052405,-0.0795845181448066,
4.41290512779767));
#8092=CARTESIAN_POINT('Ctrl Pts',(0.169837906208537,-0.0872791387223185,
4.42132666919584));
#8093=CARTESIAN_POINT('Ctrl Pts',(0.153087723973769,-0.0974871089174112,
4.43941624508146));
#8094=CARTESIAN_POINT('Ctrl Pts',(0.143800248184141,-0.1,4.44907502386883));
#8095=CARTESIAN_POINT('Ctrl Pts',(0.126030286038878,-0.1,4.46684498601409));
#8096=CARTESIAN_POINT('Ctrl Pts',(0.116371507251512,-0.0974871089174112,
4.47613246180372));
#8097=CARTESIAN_POINT('Ctrl Pts',(0.0982819313658845,-0.0872791387223186,
4.49288264403849));
#8098=CARTESIAN_POINT('Ctrl Pts',(0.0898603899677177,-0.0795845181448066,
4.50035562288236));
#8099=CARTESIAN_POINT('Ctrl Pts',(0.0764212971074882,-0.0618368682969034,
4.51201549713728));
#8100=CARTESIAN_POINT('Ctrl Pts',(0.070507117578452,-0.0505977320073438,
4.51698318771716));
#8101=CARTESIAN_POINT('Ctrl Pts',(0.0626216569908498,-0.0259622584309891,
4.52353400190554));
#8102=CARTESIAN_POINT('Ctrl Pts',(0.0606601717798219,-0.0125652179652417,
4.52512626584708));
#8103=CARTESIAN_POINT('Ctrl Pts',(0.0606601717798219,0.0125652179652417,
4.52512626584708));
#8104=CARTESIAN_POINT('Ctrl Pts',(0.0626216569908498,0.0259622584309891,
4.52353400190554));
#8105=CARTESIAN_POINT('Ctrl Pts',(0.070507117578452,0.0505977320073438,
4.51698318771716));
#8106=CARTESIAN_POINT('Ctrl Pts',(0.0764212971074882,0.0618368682969034,
4.51201549713728));
#8107=CARTESIAN_POINT('Ctrl Pts',(0.0898603899677177,0.0795845181448066,
4.50035562288236));
#8108=CARTESIAN_POINT('Ctrl Pts',(0.0982819313658845,0.0872791387223186,
4.49288264403849));
#8109=CARTESIAN_POINT('Ctrl Pts',(0.116371507251512,0.0974871089174112,
4.47613246180372));
#8110=CARTESIAN_POINT('Ctrl Pts',(0.126030286038878,0.1,4.46684498601409));
#8111=CARTESIAN_POINT('Ctrl Pts',(0.134915267111509,0.1,4.45796000494146));
#8112=CARTESIAN_POINT('',(0.131370849898476,-1.22464679914735E-17,4.31299423149112));
#8113=CARTESIAN_POINT('',(1.75771644662754,-1.22464679914735E-17,5.93933982822018));
#8114=CARTESIAN_POINT('',(0.0638809618435405,0.1,4.38692569967349));
#8115=CARTESIAN_POINT('Ctrl Pts',(0.063880961843541,0.1,4.38692569967349));
#8116=CARTESIAN_POINT('Ctrl Pts',(0.0549970964695356,0.1,4.3958095650475));
#8117=CARTESIAN_POINT('Ctrl Pts',(0.0453558658858872,0.0974877239801243,
4.40511363933968));
#8118=CARTESIAN_POINT('Ctrl Pts',(0.0273273358851931,0.0872802053318254,
4.42192548993835));
#8119=CARTESIAN_POINT('Ctrl Pts',(0.0189484612814899,0.0795853421796021,
4.42944252883495));
#8120=CARTESIAN_POINT('Ctrl Pts',(0.00558934676600131,0.0618360346560357,
4.44118472574202));
#8121=CARTESIAN_POINT('Ctrl Pts',(-0.000281894107977299,0.050595917361617,
4.44619568736696));
#8122=CARTESIAN_POINT('Ctrl Pts',(-0.00810626685067395,0.025960017775146,
4.45280694304218));
#8123=CARTESIAN_POINT('Ctrl Pts',(-0.010050506338833,0.0125636537375776,
4.45441558772843));
#8124=CARTESIAN_POINT('Ctrl Pts',(-0.010050506338833,-0.0125636537375777,
4.45441558772843));
#8125=CARTESIAN_POINT('Ctrl Pts',(-0.00810626685067328,-0.0259600177751462,
4.45280694304218));
#8126=CARTESIAN_POINT('Ctrl Pts',(-0.000281894107976854,-0.0505959173616172,
4.44619568736696));
#8127=CARTESIAN_POINT('Ctrl Pts',(0.00558934676600176,-0.0618360346560357,
4.44118472574202));
#8128=CARTESIAN_POINT('Ctrl Pts',(0.0189484612814903,-0.0795853421796021,
4.42944252883495));
#8129=CARTESIAN_POINT('Ctrl Pts',(0.027327335885194,-0.0872802053318259,
4.42192548993835));
#8130=CARTESIAN_POINT('Ctrl Pts',(0.0453558658858877,-0.0974877239801243,
4.40511363933968));
#8131=CARTESIAN_POINT('Ctrl Pts',(0.0549970964695354,-0.1,4.3958095650475));
#8132=CARTESIAN_POINT('Ctrl Pts',(0.0727648272175463,-0.1,4.37804183429949));
#8133=CARTESIAN_POINT('Ctrl Pts',(0.0820689015097318,-0.0974877239801243,
4.36840060371584));
#8134=CARTESIAN_POINT('Ctrl Pts',(0.0988807521083963,-0.0872802053318254,
4.35037207371515));
#8135=CARTESIAN_POINT('Ctrl Pts',(0.106397791004994,-0.0795853421796022,
4.34199319911144));
#8136=CARTESIAN_POINT('Ctrl Pts',(0.118139987912063,-0.0618360346560357,
4.32863408459595));
#8137=CARTESIAN_POINT('Ctrl Pts',(0.123150949537006,-0.050595917361617,
4.32276284372197));
#8138=CARTESIAN_POINT('Ctrl Pts',(0.129762205212228,-0.025960017775146,
4.31493847097928));
#8139=CARTESIAN_POINT('Ctrl Pts',(0.131370849898477,-0.0125636537375777,
4.31299423149112));
#8140=CARTESIAN_POINT('Ctrl Pts',(0.131370849898477,-1.73472347597681E-17,
4.31299423149112));
#8141=CARTESIAN_POINT('Ctrl Pts',(0.131370849898477,1.38777878078145E-17,
4.31299423149112));
#8142=CARTESIAN_POINT('Ctrl Pts',(0.131370849898477,0.0125636537375777,
4.31299423149112));
#8143=CARTESIAN_POINT('Ctrl Pts',(0.129762205212228,0.0259600177751461,
4.31493847097928));
#8144=CARTESIAN_POINT('Ctrl Pts',(0.123150949537006,0.050595917361617,4.32276284372197));
#8145=CARTESIAN_POINT('Ctrl Pts',(0.118139987912063,0.0618360346560357,
4.32863408459595));
#8146=CARTESIAN_POINT('Ctrl Pts',(0.106397791004993,0.0795853421796021,
4.34199319911144));
#8147=CARTESIAN_POINT('Ctrl Pts',(0.0988807521083954,0.0872802053318259,
4.35037207371515));
#8148=CARTESIAN_POINT('Ctrl Pts',(0.0820689015097313,0.0974877239801243,
4.36840060371584));
#8149=CARTESIAN_POINT('Ctrl Pts',(0.0727648272175463,0.1,4.37804183429949));
#8150=CARTESIAN_POINT('Ctrl Pts',(0.0638809618435408,0.1,4.38692569967349));
#8151=CARTESIAN_POINT('Origin',(1.12132034355964,0.,6.57573593128807));
#8152=CARTESIAN_POINT('',(1.04738887537727,0.1,6.5018044631057));
#8153=CARTESIAN_POINT('',(1.12132034355964,-1.22464679914735E-17,6.43431457505076));
#8154=CARTESIAN_POINT('Ctrl Pts',(1.04738887537727,0.1,6.5018044631057));
#8155=CARTESIAN_POINT('Ctrl Pts',(1.05627274075127,0.1,6.49292059773169));
#8156=CARTESIAN_POINT('Ctrl Pts',(1.06591397133492,0.0974877239801243,6.48361652343951));
#8157=CARTESIAN_POINT('Ctrl Pts',(1.08394250133562,0.0872802053318253,6.46680467284084));
#8158=CARTESIAN_POINT('Ctrl Pts',(1.09232137593932,0.0795853421796021,6.45928763394425));
#8159=CARTESIAN_POINT('Ctrl Pts',(1.10568049045481,0.0618360346560357,6.44754543703718));
#8160=CARTESIAN_POINT('Ctrl Pts',(1.11155173132879,0.0505959173616168,6.44253447541223));
#8161=CARTESIAN_POINT('Ctrl Pts',(1.11937610407148,0.0259600177751459,6.43592321973701));
#8162=CARTESIAN_POINT('Ctrl Pts',(1.12132034355964,0.0125636537375777,6.43431457505076));
#8163=CARTESIAN_POINT('Ctrl Pts',(1.12132034355964,4.5102810375397E-17,
6.43431457505076));
#8164=CARTESIAN_POINT('',(0.979898987322333,-1.26336172136316E-16,6.57573593128807));
#8165=CARTESIAN_POINT('Ctrl Pts',(0.979898987322333,-1.52655665885959E-16,
6.57573593128807));
#8166=CARTESIAN_POINT('Ctrl Pts',(0.979898987322333,0.0125636537375775,
6.57573593128807));
#8167=CARTESIAN_POINT('Ctrl Pts',(0.981507632008582,0.0259600177751462,
6.57379169179991));
#8168=CARTESIAN_POINT('Ctrl Pts',(0.988118887683804,0.0505959173616171,
6.56596731905722));
#8169=CARTESIAN_POINT('Ctrl Pts',(0.993129849308747,0.0618360346560358,
6.56009607818324));
#8170=CARTESIAN_POINT('Ctrl Pts',(1.00487204621582,0.0795853421796022,6.54673696366775));
#8171=CARTESIAN_POINT('Ctrl Pts',(1.01238908511241,0.0872802053318251,6.53835808906405));
#8172=CARTESIAN_POINT('Ctrl Pts',(1.02920093571108,0.0974877239801242,6.52032955906335));
#8173=CARTESIAN_POINT('Ctrl Pts',(1.03850501000326,0.1,6.5106883284797));
#8174=CARTESIAN_POINT('Ctrl Pts',(1.04738887537727,0.1,6.5018044631057));
#8175=CARTESIAN_POINT('Ctrl Pts',(1.12132034355964,-3.46944695195361E-18,
6.43431457505076));
#8176=CARTESIAN_POINT('Ctrl Pts',(1.12132034355964,-0.0125636537375777,
6.43431457505076));
#8177=CARTESIAN_POINT('Ctrl Pts',(1.11937610407148,-0.0259600177751459,
6.43592321973701));
#8178=CARTESIAN_POINT('Ctrl Pts',(1.11155173132879,-0.0505959173616168,
6.44253447541223));
#8179=CARTESIAN_POINT('Ctrl Pts',(1.10568049045481,-0.0618360346560357,
6.44754543703718));
#8180=CARTESIAN_POINT('Ctrl Pts',(1.09232137593932,-0.0795853421796021,
6.45928763394425));
#8181=CARTESIAN_POINT('Ctrl Pts',(1.08394250133562,-0.0872802053318253,
6.46680467284084));
#8182=CARTESIAN_POINT('Ctrl Pts',(1.06591397133492,-0.0974877239801243,
6.48361652343951));
#8183=CARTESIAN_POINT('Ctrl Pts',(1.05627274075127,-0.1,6.49292059773169));
#8184=CARTESIAN_POINT('Ctrl Pts',(1.03850501000326,-0.1,6.5106883284797));
#8185=CARTESIAN_POINT('Ctrl Pts',(1.02920093571108,-0.0974877239801243,
6.52032955906335));
#8186=CARTESIAN_POINT('Ctrl Pts',(1.01238908511241,-0.0872802053318255,
6.53835808906405));
#8187=CARTESIAN_POINT('Ctrl Pts',(1.00487204621582,-0.0795853421796022,
6.54673696366775));
#8188=CARTESIAN_POINT('Ctrl Pts',(0.993129849308747,-0.0618360346560358,
6.56009607818324));
#8189=CARTESIAN_POINT('Ctrl Pts',(0.988118887683804,-0.0505959173616169,
6.56596731905722));
#8190=CARTESIAN_POINT('Ctrl Pts',(0.981507632008582,-0.025960017775146,
6.57379169179991));
#8191=CARTESIAN_POINT('Ctrl Pts',(0.979898987322333,-0.0125636537375777,
6.57573593128807));
#8192=CARTESIAN_POINT('Ctrl Pts',(0.979898987322333,-2.42861286636753E-17,
6.57573593128807));
#8193=CARTESIAN_POINT('',(1.05060966544099,-6.12323399573679E-18,6.36360389693211));
#8194=CARTESIAN_POINT('',(1.1920310216783,-1.22464679914735E-17,6.50502525316942));
#8195=CARTESIAN_POINT('',(0.909188309203678,-5.42934460534604E-17,6.50502525316942));
#8196=CARTESIAN_POINT('Ctrl Pts',(0.909188309203678,1.73472347597681E-17,
6.50502525316942));
#8197=CARTESIAN_POINT('Ctrl Pts',(0.909188309203678,-0.0125652179652416,
6.50502525316942));
#8198=CARTESIAN_POINT('Ctrl Pts',(0.910780573145226,-0.0259622584309893,
6.50306376795839));
#8199=CARTESIAN_POINT('Ctrl Pts',(0.917331387333598,-0.0505977320073438,
6.49517830737079));
#8200=CARTESIAN_POINT('Ctrl Pts',(0.922299077913481,-0.0618368682969034,
6.48926412784175));
#8201=CARTESIAN_POINT('Ctrl Pts',(0.933958952168405,-0.0795845181448066,
6.47582503498152));
#8202=CARTESIAN_POINT('Ctrl Pts',(0.941431931012273,-0.0872791387223182,
6.46740349358335));
#8203=CARTESIAN_POINT('Ctrl Pts',(0.958182113247041,-0.0974871089174111,
6.44931391769773));
#8204=CARTESIAN_POINT('Ctrl Pts',(0.967469589036669,-0.1,6.43965513891036));
#8205=CARTESIAN_POINT('Ctrl Pts',(0.985239551181931,-0.1,6.4218851767651));
#8206=CARTESIAN_POINT('Ctrl Pts',(0.994898329969298,-0.097487108917411,
6.41259770097547));
#8207=CARTESIAN_POINT('Ctrl Pts',(1.01298790585493,-0.0872791387223182,
6.3958475187407));
#8208=CARTESIAN_POINT('Ctrl Pts',(1.02140944725309,-0.0795845181448066,
6.38837453989683));
#8209=CARTESIAN_POINT('Ctrl Pts',(1.03484854011332,-0.0618368682969034,
6.37671466564191));
#8210=CARTESIAN_POINT('Ctrl Pts',(1.04076271964236,-0.0505977320073438,
6.37174697506203));
#8211=CARTESIAN_POINT('Ctrl Pts',(1.04864818022996,-0.0259622584309893,
6.36519616087365));
#8212=CARTESIAN_POINT('Ctrl Pts',(1.05060966544099,-0.0125652179652416,
6.36360389693211));
#8213=CARTESIAN_POINT('Ctrl Pts',(1.05060966544099,-1.38777878078145E-17,
6.36360389693211));
#8214=CARTESIAN_POINT('',(0.9763545701093,0.1,6.43077015783773));
#8215=CARTESIAN_POINT('Ctrl Pts',(0.9763545701093,0.1,6.43077015783773));
#8216=CARTESIAN_POINT('Ctrl Pts',(0.967469589036669,0.1,6.43965513891036));
#8217=CARTESIAN_POINT('Ctrl Pts',(0.958182113247041,0.0974871089174111,
6.44931391769773));
#8218=CARTESIAN_POINT('Ctrl Pts',(0.941431931012273,0.0872791387223182,
6.46740349358335));
#8219=CARTESIAN_POINT('Ctrl Pts',(0.933958952168405,0.0795845181448066,
6.47582503498152));
#8220=CARTESIAN_POINT('Ctrl Pts',(0.922299077913481,0.0618368682969034,
6.48926412784175));
#8221=CARTESIAN_POINT('Ctrl Pts',(0.917331387333598,0.0505977320073438,
6.49517830737079));
#8222=CARTESIAN_POINT('Ctrl Pts',(0.910780573145226,0.0259622584309893,
6.50306376795839));
#8223=CARTESIAN_POINT('Ctrl Pts',(0.909188309203678,0.0125652179652416,
6.50502525316942));
#8224=CARTESIAN_POINT('Ctrl Pts',(0.909188309203678,6.93889390390723E-18,
6.50502525316942));
#8225=CARTESIAN_POINT('Ctrl Pts',(1.05060966544099,-2.77555756156289E-17,
6.36360389693211));
#8226=CARTESIAN_POINT('Ctrl Pts',(1.05060966544099,0.0125652179652416,6.36360389693211));
#8227=CARTESIAN_POINT('Ctrl Pts',(1.04864818022996,0.0259622584309892,6.36519616087365));
#8228=CARTESIAN_POINT('Ctrl Pts',(1.04076271964236,0.0505977320073438,6.37174697506203));
#8229=CARTESIAN_POINT('Ctrl Pts',(1.03484854011332,0.0618368682969034,6.37671466564191));
#8230=CARTESIAN_POINT('Ctrl Pts',(1.02140944725309,0.0795845181448066,6.38837453989683));
#8231=CARTESIAN_POINT('Ctrl Pts',(1.01298790585493,0.0872791387223182,6.3958475187407));
#8232=CARTESIAN_POINT('Ctrl Pts',(0.994898329969298,0.0974871089174111,
6.41259770097547));
#8233=CARTESIAN_POINT('Ctrl Pts',(0.985239551181931,0.1,6.4218851767651));
#8234=CARTESIAN_POINT('Ctrl Pts',(0.9763545701093,0.1,6.43077015783773));
#8235=CARTESIAN_POINT('Origin',(1.12132034355964,0.,6.57573593128807));
#8236=CARTESIAN_POINT('',(-0.430770157837729,0.1,5.0236454298907));
#8237=CARTESIAN_POINT('',(-0.363603896932107,-2.65378704378315E-18,4.94939033455901));
#8238=CARTESIAN_POINT('Ctrl Pts',(-0.430770157837728,0.1,5.0236454298907));
#8239=CARTESIAN_POINT('Ctrl Pts',(-0.421885176765097,0.1,5.01476044881807));
#8240=CARTESIAN_POINT('Ctrl Pts',(-0.412597700975469,0.0974871089174111,
5.0051016700307));
#8241=CARTESIAN_POINT('Ctrl Pts',(-0.395847518740701,0.0872791387223182,
4.98701209414507));
#8242=CARTESIAN_POINT('Ctrl Pts',(-0.388374539896833,0.0795845181448066,
4.97859055274691));
#8243=CARTESIAN_POINT('Ctrl Pts',(-0.37671466564191,0.0618368682969034,
4.96515145988668));
#8244=CARTESIAN_POINT('Ctrl Pts',(-0.371746975062027,0.0505977320073438,
4.95923728035764));
#8245=CARTESIAN_POINT('Ctrl Pts',(-0.365196160873654,0.0259622584309892,
4.95135181977004));
#8246=CARTESIAN_POINT('Ctrl Pts',(-0.363603896932107,0.0125652179652416,
4.94939033455901));
#8247=CARTESIAN_POINT('Ctrl Pts',(-0.363603896932107,-3.46944695195361E-18,
4.94939033455901));
#8248=CARTESIAN_POINT('Ctrl Pts',(-0.363603896932107,-2.77555756156289E-17,
4.94939033455901));
#8249=CARTESIAN_POINT('Ctrl Pts',(-0.363603896932107,-0.0125652179652417,
4.94939033455901));
#8250=CARTESIAN_POINT('Ctrl Pts',(-0.365196160873654,-0.0259622584309891,
4.95135181977004));
#8251=CARTESIAN_POINT('Ctrl Pts',(-0.371746975062026,-0.0505977320073437,
4.95923728035764));
#8252=CARTESIAN_POINT('Ctrl Pts',(-0.376714665641909,-0.0618368682969034,
4.96515145988668));
#8253=CARTESIAN_POINT('Ctrl Pts',(-0.388374539896833,-0.0795845181448066,
4.97859055274691));
#8254=CARTESIAN_POINT('Ctrl Pts',(-0.395847518740701,-0.087279138722318,
4.98701209414507));
#8255=CARTESIAN_POINT('Ctrl Pts',(-0.412597700975469,-0.0974871089174109,
5.0051016700307));
#8256=CARTESIAN_POINT('Ctrl Pts',(-0.421885176765097,-0.1,5.01476044881807));
#8257=CARTESIAN_POINT('Ctrl Pts',(-0.43965513891036,-0.1,5.03253041096333));
#8258=CARTESIAN_POINT('Ctrl Pts',(-0.449313917697726,-0.0974871089174111,
5.04181788675296));
#8259=CARTESIAN_POINT('Ctrl Pts',(-0.467403493583354,-0.0872791387223182,
5.05856806898773));
#8260=CARTESIAN_POINT('Ctrl Pts',(-0.475825034981521,-0.0795845181448066,
5.06604104783159));
#8261=CARTESIAN_POINT('Ctrl Pts',(-0.48926412784175,-0.0618368682969034,
5.07770092208652));
#8262=CARTESIAN_POINT('Ctrl Pts',(-0.495178307370786,-0.0505977320073439,
5.0826686126664));
#8263=CARTESIAN_POINT('Ctrl Pts',(-0.503063767958388,-0.0259622584309893,
5.08921942685477));
#8264=CARTESIAN_POINT('Ctrl Pts',(-0.505025253169416,-0.0125652179652416,
5.09081169079632));
#8265=CARTESIAN_POINT('Ctrl Pts',(-0.505025253169416,0.0125652179652416,
5.09081169079632));
#8266=CARTESIAN_POINT('Ctrl Pts',(-0.503063767958388,0.0259622584309892,
5.08921942685477));
#8267=CARTESIAN_POINT('Ctrl Pts',(-0.495178307370786,0.0505977320073437,
5.0826686126664));
#8268=CARTESIAN_POINT('Ctrl Pts',(-0.48926412784175,0.0618368682969034,
5.07770092208652));
#8269=CARTESIAN_POINT('Ctrl Pts',(-0.475825034981521,0.0795845181448066,
5.06604104783159));
#8270=CARTESIAN_POINT('Ctrl Pts',(-0.467403493583354,0.0872791387223182,
5.05856806898773));
#8271=CARTESIAN_POINT('Ctrl Pts',(-0.449313917697726,0.0974871089174111,
5.04181788675296));
#8272=CARTESIAN_POINT('Ctrl Pts',(-0.439655138910359,0.1,5.03253041096333));
#8273=CARTESIAN_POINT('Ctrl Pts',(-0.430770157837728,0.1,5.0236454298907));
#8274=CARTESIAN_POINT('',(-0.434314575050762,-1.22464679914735E-17,4.87867965644036));
#8275=CARTESIAN_POINT('',(1.1920310216783,-1.22464679914735E-17,6.50502525316942));
#8276=CARTESIAN_POINT('',(-0.501804463105697,0.1,4.95261112462273));
#8277=CARTESIAN_POINT('Ctrl Pts',(-0.501804463105697,0.1,4.95261112462273));
#8278=CARTESIAN_POINT('Ctrl Pts',(-0.510688328479703,0.1,4.96149498999674));
#8279=CARTESIAN_POINT('Ctrl Pts',(-0.520329559063351,0.0974877239801243,
4.97079906428892));
#8280=CARTESIAN_POINT('Ctrl Pts',(-0.538358089064045,0.0872802053318253,
4.98761091488759));
#8281=CARTESIAN_POINT('Ctrl Pts',(-0.546736963667748,0.0795853421796022,
4.99512795378418));
#8282=CARTESIAN_POINT('Ctrl Pts',(-0.560096078183237,0.0618360346560358,
5.00687015069125));
#8283=CARTESIAN_POINT('Ctrl Pts',(-0.565967319057215,0.0505959173616169,
5.0118811123162));
#8284=CARTESIAN_POINT('Ctrl Pts',(-0.573791691799912,0.025960017775146,
5.01849236799142));
#8285=CARTESIAN_POINT('Ctrl Pts',(-0.575735931288071,0.0125636537375776,
5.02010101267767));
#8286=CARTESIAN_POINT('Ctrl Pts',(-0.575735931288071,-0.0125636537375777,
5.02010101267767));
#8287=CARTESIAN_POINT('Ctrl Pts',(-0.573791691799912,-0.025960017775146,
5.01849236799142));
#8288=CARTESIAN_POINT('Ctrl Pts',(-0.565967319057215,-0.0505959173616169,
5.0118811123162));
#8289=CARTESIAN_POINT('Ctrl Pts',(-0.560096078183237,-0.0618360346560358,
5.00687015069125));
#8290=CARTESIAN_POINT('Ctrl Pts',(-0.546736963667748,-0.0795853421796022,
4.99512795378418));
#8291=CARTESIAN_POINT('Ctrl Pts',(-0.538358089064045,-0.0872802053318255,
4.98761091488759));
#8292=CARTESIAN_POINT('Ctrl Pts',(-0.52032955906335,-0.0974877239801243,
4.97079906428892));
#8293=CARTESIAN_POINT('Ctrl Pts',(-0.510688328479703,-0.1,4.96149498999674));
#8294=CARTESIAN_POINT('Ctrl Pts',(-0.492920597731692,-0.1,4.94372725924873));
#8295=CARTESIAN_POINT('Ctrl Pts',(-0.483616523439507,-0.0974877239801243,
4.93408602866508));
#8296=CARTESIAN_POINT('Ctrl Pts',(-0.466804672840842,-0.0872802053318253,
4.91605749866438));
#8297=CARTESIAN_POINT('Ctrl Pts',(-0.459287633944245,-0.0795853421796021,
4.90767862406068));
#8298=CARTESIAN_POINT('Ctrl Pts',(-0.447545437037175,-0.0618360346560357,
4.89431950954519));
#8299=CARTESIAN_POINT('Ctrl Pts',(-0.442534475412232,-0.0505959173616168,
4.88844826867121));
#8300=CARTESIAN_POINT('Ctrl Pts',(-0.43592321973701,-0.0259600177751459,
4.88062389592852));
#8301=CARTESIAN_POINT('Ctrl Pts',(-0.434314575050762,-0.0125636537375777,
4.87867965644036));
#8302=CARTESIAN_POINT('Ctrl Pts',(-0.434314575050762,-1.73472347597681E-17,
4.87867965644036));
#8303=CARTESIAN_POINT('Ctrl Pts',(-0.434314575050762,2.77555756156289E-17,
4.87867965644036));
#8304=CARTESIAN_POINT('Ctrl Pts',(-0.434314575050762,0.0125636537375777,
4.87867965644036));
#8305=CARTESIAN_POINT('Ctrl Pts',(-0.43592321973701,0.0259600177751459,
4.88062389592852));
#8306=CARTESIAN_POINT('Ctrl Pts',(-0.442534475412232,0.0505959173616168,
4.88844826867121));
#8307=CARTESIAN_POINT('Ctrl Pts',(-0.447545437037175,0.0618360346560357,
4.89431950954519));
#8308=CARTESIAN_POINT('Ctrl Pts',(-0.459287633944245,0.0795853421796021,
4.90767862406068));
#8309=CARTESIAN_POINT('Ctrl Pts',(-0.466804672840842,0.0872802053318255,
4.91605749866438));
#8310=CARTESIAN_POINT('Ctrl Pts',(-0.483616523439507,0.0974877239801244,
4.93408602866508));
#8311=CARTESIAN_POINT('Ctrl Pts',(-0.492920597731692,0.1,4.94372725924873));
#8312=CARTESIAN_POINT('Ctrl Pts',(-0.501804463105698,0.1,4.95261112462273));
#8313=CARTESIAN_POINT('Origin',(3.3840620433566,0.,4.31299423149112));
#8314=CARTESIAN_POINT('',(3.31013057517422,0.0999999999999996,4.23906276330875));
#8315=CARTESIAN_POINT('',(3.3840620433566,-1.22464679914735E-17,4.17157287525381));
#8316=CARTESIAN_POINT('Ctrl Pts',(3.31013057517422,0.0999999999999996,4.23906276330875));
#8317=CARTESIAN_POINT('Ctrl Pts',(3.31901444054823,0.0999999999999996,4.23017889793474));
#8318=CARTESIAN_POINT('Ctrl Pts',(3.32865567113187,0.0974877239801239,4.22087482364256));
#8319=CARTESIAN_POINT('Ctrl Pts',(3.34668420113257,0.0872802053318249,4.20406297304389));
#8320=CARTESIAN_POINT('Ctrl Pts',(3.35506307573627,0.0795853421796018,4.19654593414729));
#8321=CARTESIAN_POINT('Ctrl Pts',(3.36842219025176,0.0618360346560355,4.18480373724022));
#8322=CARTESIAN_POINT('Ctrl Pts',(3.37429343112574,0.0505959173616165,4.17979277561528));
#8323=CARTESIAN_POINT('Ctrl Pts',(3.38211780386844,0.0259600177751457,4.17318151994006));
#8324=CARTESIAN_POINT('Ctrl Pts',(3.3840620433566,0.0125636537375776,4.17157287525381));
#8325=CARTESIAN_POINT('Ctrl Pts',(3.3840620433566,-1.38777878078145E-17,
4.17157287525381));
#8326=CARTESIAN_POINT('',(3.24264068711929,-9.68458730447101E-17,4.31299423149112));
#8327=CARTESIAN_POINT('Ctrl Pts',(3.24264068711929,-5.20417042793042E-17,
4.31299423149112));
#8328=CARTESIAN_POINT('Ctrl Pts',(3.24264068711929,0.0125636537375775,4.31299423149112));
#8329=CARTESIAN_POINT('Ctrl Pts',(3.24424933180553,0.0259600177751457,4.31104999200296));
#8330=CARTESIAN_POINT('Ctrl Pts',(3.25086058748076,0.0505959173616165,4.30322561926026));
#8331=CARTESIAN_POINT('Ctrl Pts',(3.2558715491057,0.0618360346560354,4.29735437838629));
#8332=CARTESIAN_POINT('Ctrl Pts',(3.26761374601277,0.0795853421796018,4.2839952638708));
#8333=CARTESIAN_POINT('Ctrl Pts',(3.27513078490937,0.0872802053318246,4.27561638926709));
#8334=CARTESIAN_POINT('Ctrl Pts',(3.29194263550803,0.0974877239801235,4.2575878592664));
#8335=CARTESIAN_POINT('Ctrl Pts',(3.30124670980022,0.0999999999999997,4.24794662868275));
#8336=CARTESIAN_POINT('Ctrl Pts',(3.31013057517422,0.0999999999999997,4.23906276330875));
#8337=CARTESIAN_POINT('Ctrl Pts',(3.3840620433566,-4.16333634234434E-17,
4.17157287525381));
#8338=CARTESIAN_POINT('Ctrl Pts',(3.3840620433566,-0.0125636537375776,4.17157287525381));
#8339=CARTESIAN_POINT('Ctrl Pts',(3.38211780386844,-0.0259600177751457,
4.17318151994006));
#8340=CARTESIAN_POINT('Ctrl Pts',(3.37429343112574,-0.0505959173616165,
4.17979277561528));
#8341=CARTESIAN_POINT('Ctrl Pts',(3.36842219025176,-0.0618360346560354,
4.18480373724022));
#8342=CARTESIAN_POINT('Ctrl Pts',(3.35506307573627,-0.0795853421796018,
4.19654593414729));
#8343=CARTESIAN_POINT('Ctrl Pts',(3.34668420113257,-0.0872802053318246,
4.20406297304389));
#8344=CARTESIAN_POINT('Ctrl Pts',(3.32865567113188,-0.0974877239801235,
4.22087482364255));
#8345=CARTESIAN_POINT('Ctrl Pts',(3.31901444054823,-0.0999999999999996,
4.23017889793474));
#8346=CARTESIAN_POINT('Ctrl Pts',(3.30124670980022,-0.0999999999999996,
4.24794662868275));
#8347=CARTESIAN_POINT('Ctrl Pts',(3.29194263550803,-0.0974877239801242,
4.2575878592664));
#8348=CARTESIAN_POINT('Ctrl Pts',(3.27513078490937,-0.0872802053318254,
4.27561638926709));
#8349=CARTESIAN_POINT('Ctrl Pts',(3.26761374601277,-0.0795853421796018,
4.2839952638708));
#8350=CARTESIAN_POINT('Ctrl Pts',(3.2558715491057,-0.0618360346560355,4.29735437838629));
#8351=CARTESIAN_POINT('Ctrl Pts',(3.25086058748076,-0.0505959173616171,
4.30322561926026));
#8352=CARTESIAN_POINT('Ctrl Pts',(3.24424933180553,-0.0259600177751463,
4.31104999200296));
#8353=CARTESIAN_POINT('Ctrl Pts',(3.24264068711929,-0.0125636537375776,
4.31299423149112));
#8354=CARTESIAN_POINT('Ctrl Pts',(3.24264068711929,-3.46944695195361E-17,
4.31299423149112));
#8355=CARTESIAN_POINT('',(3.31335136523794,-7.85795747171355E-18,4.10086219713516));
#8356=CARTESIAN_POINT('',(3.45477272147525,-1.22464679914735E-17,4.24228355337247));
#8357=CARTESIAN_POINT('',(3.17193000900063,-7.51101277651821E-17,4.24228355337246));
#8358=CARTESIAN_POINT('Ctrl Pts',(3.17193000900063,-2.08166817117217E-17,
4.24228355337246));
#8359=CARTESIAN_POINT('Ctrl Pts',(3.17193000900063,-0.0125652179652416,
4.24228355337246));
#8360=CARTESIAN_POINT('Ctrl Pts',(3.17352227294218,-0.025962258430989,4.24032206816144));
#8361=CARTESIAN_POINT('Ctrl Pts',(3.18007308713055,-0.0505977320073433,
4.23243660757383));
#8362=CARTESIAN_POINT('Ctrl Pts',(3.18504077771043,-0.0618368682969031,
4.2265224280448));
#8363=CARTESIAN_POINT('Ctrl Pts',(3.19670065196536,-0.0795845181448063,
4.21308333518457));
#8364=CARTESIAN_POINT('Ctrl Pts',(3.20417363080922,-0.0872791387223176,
4.2046617937864));
#8365=CARTESIAN_POINT('Ctrl Pts',(3.22092381304399,-0.0974871089174107,
4.18657221790077));
#8366=CARTESIAN_POINT('Ctrl Pts',(3.23021128883362,-0.0999999999999996,
4.17691343911341));
#8367=CARTESIAN_POINT('Ctrl Pts',(3.24798125097888,-0.0999999999999996,
4.15914347696815));
#8368=CARTESIAN_POINT('Ctrl Pts',(3.25764002976625,-0.0974871089174107,
4.14985600117852));
#8369=CARTESIAN_POINT('Ctrl Pts',(3.27572960565188,-0.0872791387223176,
4.13310581894375));
#8370=CARTESIAN_POINT('Ctrl Pts',(3.28415114705005,-0.0795845181448063,
4.12563284009988));
#8371=CARTESIAN_POINT('Ctrl Pts',(3.29759023991027,-0.0618368682969031,
4.11397296584496));
#8372=CARTESIAN_POINT('Ctrl Pts',(3.30350441943931,-0.0505977320073432,
4.10900527526508));
#8373=CARTESIAN_POINT('Ctrl Pts',(3.31138988002691,-0.025962258430989,4.1024544610767));
#8374=CARTESIAN_POINT('Ctrl Pts',(3.31335136523794,-0.0125652179652416,
4.10086219713516));
#8375=CARTESIAN_POINT('Ctrl Pts',(3.31335136523794,-3.12250225675825E-17,
4.10086219713516));
#8376=CARTESIAN_POINT('',(3.23909626990625,0.0999999999999996,4.16802845804078));
#8377=CARTESIAN_POINT('Ctrl Pts',(3.23909626990625,0.0999999999999996,4.16802845804078));
#8378=CARTESIAN_POINT('Ctrl Pts',(3.23021128883362,0.0999999999999997,4.17691343911341));
#8379=CARTESIAN_POINT('Ctrl Pts',(3.22092381304399,0.0974871089174107,4.18657221790077));
#8380=CARTESIAN_POINT('Ctrl Pts',(3.20417363080922,0.0872791387223176,4.2046617937864));
#8381=CARTESIAN_POINT('Ctrl Pts',(3.19670065196536,0.0795845181448063,4.21308333518457));
#8382=CARTESIAN_POINT('Ctrl Pts',(3.18504077771043,0.0618368682969031,4.2265224280448));
#8383=CARTESIAN_POINT('Ctrl Pts',(3.18007308713055,0.0505977320073433,4.23243660757383));
#8384=CARTESIAN_POINT('Ctrl Pts',(3.17352227294218,0.0259622584309891,4.24032206816144));
#8385=CARTESIAN_POINT('Ctrl Pts',(3.17193000900063,0.0125652179652416,4.24228355337246));
#8386=CARTESIAN_POINT('Ctrl Pts',(3.17193000900063,6.93889390390723E-17,
4.24228355337246));
#8387=CARTESIAN_POINT('Ctrl Pts',(3.31335136523794,1.38777878078145E-17,
4.10086219713516));
#8388=CARTESIAN_POINT('Ctrl Pts',(3.31335136523794,0.0125652179652416,4.10086219713516));
#8389=CARTESIAN_POINT('Ctrl Pts',(3.31138988002691,0.0259622584309891,4.1024544610767));
#8390=CARTESIAN_POINT('Ctrl Pts',(3.30350441943931,0.0505977320073433,4.10900527526507));
#8391=CARTESIAN_POINT('Ctrl Pts',(3.29759023991027,0.0618368682969031,4.11397296584496));
#8392=CARTESIAN_POINT('Ctrl Pts',(3.28415114705005,0.0795845181448063,4.12563284009988));
#8393=CARTESIAN_POINT('Ctrl Pts',(3.27572960565188,0.0872791387223176,4.13310581894375));
#8394=CARTESIAN_POINT('Ctrl Pts',(3.25764002976625,0.0974871089174107,4.14985600117852));
#8395=CARTESIAN_POINT('Ctrl Pts',(3.24798125097888,0.0999999999999996,4.15914347696815));
#8396=CARTESIAN_POINT('Ctrl Pts',(3.23909626990625,0.0999999999999996,4.16802845804078));
#8397=CARTESIAN_POINT('Origin',(3.3840620433566,0.,4.31299423149112));
#8398=CARTESIAN_POINT('',(1.83197154195922,0.0999999999999996,2.76090373009375));
#8399=CARTESIAN_POINT('',(1.89913780286485,-2.00010218035512E-17,2.68664863476206));
#8400=CARTESIAN_POINT('Ctrl Pts',(1.83197154195922,0.0999999999999996,2.76090373009375));
#8401=CARTESIAN_POINT('Ctrl Pts',(1.84085652303185,0.0999999999999996,2.75201874902112));
#8402=CARTESIAN_POINT('Ctrl Pts',(1.85014399882148,0.0974871089174107,2.74235997023375));
#8403=CARTESIAN_POINT('Ctrl Pts',(1.86689418105625,0.0872791387223176,2.72427039434812));
#8404=CARTESIAN_POINT('Ctrl Pts',(1.87436715990012,0.0795845181448063,2.71584885294996));
#8405=CARTESIAN_POINT('Ctrl Pts',(1.88602703415504,0.0618368682969031,2.70240976008973));
#8406=CARTESIAN_POINT('Ctrl Pts',(1.89099472473493,0.0505977320073433,2.69649558056069));
#8407=CARTESIAN_POINT('Ctrl Pts',(1.8975455389233,0.0259622584309891,2.68861011997309));
#8408=CARTESIAN_POINT('Ctrl Pts',(1.89913780286485,0.0125652179652415,2.68664863476206));
#8409=CARTESIAN_POINT('Ctrl Pts',(1.89913780286485,-4.16333634234434E-17,
2.68664863476206));
#8410=CARTESIAN_POINT('Ctrl Pts',(1.89913780286485,-2.42861286636753E-17,
2.68664863476206));
#8411=CARTESIAN_POINT('Ctrl Pts',(1.89913780286485,-0.0125652179652416,
2.68664863476206));
#8412=CARTESIAN_POINT('Ctrl Pts',(1.8975455389233,-0.0259622584309889,2.68861011997309));
#8413=CARTESIAN_POINT('Ctrl Pts',(1.89099472473493,-0.0505977320073432,
2.69649558056069));
#8414=CARTESIAN_POINT('Ctrl Pts',(1.88602703415504,-0.0618368682969031,
2.70240976008973));
#8415=CARTESIAN_POINT('Ctrl Pts',(1.87436715990012,-0.0795845181448063,
2.71584885294996));
#8416=CARTESIAN_POINT('Ctrl Pts',(1.86689418105625,-0.087279138722317,2.72427039434812));
#8417=CARTESIAN_POINT('Ctrl Pts',(1.85014399882148,-0.0974871089174103,
2.74235997023375));
#8418=CARTESIAN_POINT('Ctrl Pts',(1.84085652303186,-0.0999999999999996,
2.75201874902112));
#8419=CARTESIAN_POINT('Ctrl Pts',(1.82308656088659,-0.0999999999999996,
2.76978871116638));
#8420=CARTESIAN_POINT('Ctrl Pts',(1.81342778209923,-0.0974871089174107,
2.77907618695601));
#8421=CARTESIAN_POINT('Ctrl Pts',(1.7953382062136,-0.0872791387223176,2.79582636919078));
#8422=CARTESIAN_POINT('Ctrl Pts',(1.78691666481543,-0.0795845181448063,
2.80329934803464));
#8423=CARTESIAN_POINT('Ctrl Pts',(1.7734775719552,-0.0618368682969031,2.81495922228957));
#8424=CARTESIAN_POINT('Ctrl Pts',(1.76756339242617,-0.0505977320073433,
2.81992691286945));
#8425=CARTESIAN_POINT('Ctrl Pts',(1.75967793183856,-0.0259622584309891,
2.82647772705782));
#8426=CARTESIAN_POINT('Ctrl Pts',(1.75771644662754,-0.0125652179652416,
2.82806999099937));
#8427=CARTESIAN_POINT('Ctrl Pts',(1.75771644662754,0.0125652179652416,2.82806999099937));
#8428=CARTESIAN_POINT('Ctrl Pts',(1.75967793183856,0.0259622584309891,2.82647772705782));
#8429=CARTESIAN_POINT('Ctrl Pts',(1.76756339242617,0.0505977320073433,2.81992691286945));
#8430=CARTESIAN_POINT('Ctrl Pts',(1.7734775719552,0.0618368682969031,2.81495922228957));
#8431=CARTESIAN_POINT('Ctrl Pts',(1.78691666481543,0.0795845181448063,2.80329934803464));
#8432=CARTESIAN_POINT('Ctrl Pts',(1.7953382062136,0.0872791387223176,2.79582636919078));
#8433=CARTESIAN_POINT('Ctrl Pts',(1.81342778209923,0.0974871089174107,2.77907618695601));
#8434=CARTESIAN_POINT('Ctrl Pts',(1.82308656088659,0.0999999999999997,2.76978871116638));
#8435=CARTESIAN_POINT('Ctrl Pts',(1.83197154195922,0.0999999999999997,2.76090373009375));
#8436=CARTESIAN_POINT('',(1.82842712474619,-1.22464679914735E-17,2.61593795664341));
#8437=CARTESIAN_POINT('',(3.45477272147525,-1.22464679914735E-17,4.24228355337247));
#8438=CARTESIAN_POINT('',(1.76093723669126,0.0999999999999997,2.68986942482578));
#8439=CARTESIAN_POINT('Ctrl Pts',(1.76093723669126,0.0999999999999996,2.68986942482578));
#8440=CARTESIAN_POINT('Ctrl Pts',(1.75205337131725,0.0999999999999996,2.69875329019978));
#8441=CARTESIAN_POINT('Ctrl Pts',(1.7424121407336,0.0974877239801239,2.70805736449197));
#8442=CARTESIAN_POINT('Ctrl Pts',(1.72438361073291,0.0872802053318249,2.72486921509063));
#8443=CARTESIAN_POINT('Ctrl Pts',(1.7160047361292,0.0795853421796018,2.73238625398723));
#8444=CARTESIAN_POINT('Ctrl Pts',(1.70264562161372,0.0618360346560354,2.7441284508943));
#8445=CARTESIAN_POINT('Ctrl Pts',(1.69677438073974,0.0505959173616165,2.74913941251924));
#8446=CARTESIAN_POINT('Ctrl Pts',(1.68895000799704,0.0259600177751457,2.75575066819447));
#8447=CARTESIAN_POINT('Ctrl Pts',(1.68700576850888,0.0125636537375776,2.75735931288071));
#8448=CARTESIAN_POINT('Ctrl Pts',(1.68700576850888,-0.0125636537375776,
2.75735931288071));
#8449=CARTESIAN_POINT('Ctrl Pts',(1.68895000799704,-0.0259600177751457,
2.75575066819447));
#8450=CARTESIAN_POINT('Ctrl Pts',(1.69677438073974,-0.0505959173616166,
2.74913941251924));
#8451=CARTESIAN_POINT('Ctrl Pts',(1.70264562161372,-0.0618360346560355,
2.7441284508943));
#8452=CARTESIAN_POINT('Ctrl Pts',(1.7160047361292,-0.0795853421796018,2.73238625398723));
#8453=CARTESIAN_POINT('Ctrl Pts',(1.72438361073291,-0.0872802053318254,
2.72486921509063));
#8454=CARTESIAN_POINT('Ctrl Pts',(1.7424121407336,-0.0974877239801242,2.70805736449197));
#8455=CARTESIAN_POINT('Ctrl Pts',(1.75205337131725,-0.0999999999999996,
2.69875329019978));
#8456=CARTESIAN_POINT('Ctrl Pts',(1.76982110206526,-0.0999999999999996,
2.68098555945177));
#8457=CARTESIAN_POINT('Ctrl Pts',(1.77912517635745,-0.0974877239801239,
2.67134432886813));
#8458=CARTESIAN_POINT('Ctrl Pts',(1.79593702695611,-0.0872802053318249,
2.65331579886743));
#8459=CARTESIAN_POINT('Ctrl Pts',(1.80345406585271,-0.0795853421796018,
2.64493692426373));
#8460=CARTESIAN_POINT('Ctrl Pts',(1.81519626275978,-0.0618360346560354,
2.63157780974824));
#8461=CARTESIAN_POINT('Ctrl Pts',(1.82020722438472,-0.0505959173616165,
2.62570656887426));
#8462=CARTESIAN_POINT('Ctrl Pts',(1.82681848005994,-0.0259600177751457,
2.61788219613157));
#8463=CARTESIAN_POINT('Ctrl Pts',(1.82842712474619,-0.0125636537375776,
2.61593795664341));
#8464=CARTESIAN_POINT('Ctrl Pts',(1.82842712474619,2.08166817117217E-17,
2.61593795664341));
#8465=CARTESIAN_POINT('Ctrl Pts',(1.82842712474619,-2.77555756156289E-17,
2.61593795664341));
#8466=CARTESIAN_POINT('Ctrl Pts',(1.82842712474619,0.0125636537375776,2.61593795664341));
#8467=CARTESIAN_POINT('Ctrl Pts',(1.82681848005994,0.0259600177751457,2.61788219613157));
#8468=CARTESIAN_POINT('Ctrl Pts',(1.82020722438472,0.0505959173616165,2.62570656887426));
#8469=CARTESIAN_POINT('Ctrl Pts',(1.81519626275978,0.0618360346560355,2.63157780974824));
#8470=CARTESIAN_POINT('Ctrl Pts',(1.80345406585271,0.0795853421796018,2.64493692426373));
#8471=CARTESIAN_POINT('Ctrl Pts',(1.79593702695611,0.0872802053318249,2.65331579886743));
#8472=CARTESIAN_POINT('Ctrl Pts',(1.77912517635745,0.0974877239801239,2.67134432886813));
#8473=CARTESIAN_POINT('Ctrl Pts',(1.76982110206526,0.0999999999999996,2.68098555945177));
#8474=CARTESIAN_POINT('Ctrl Pts',(1.76093723669126,0.0999999999999996,2.68986942482578));
#8475=CARTESIAN_POINT('Origin',(3.23556961930742,0.,2.76443038069258));
#8476=CARTESIAN_POINT('',(3.72700883223207,-8.38883057415937E-17,3.2417274579935));
#8477=CARTESIAN_POINT('Origin',(3.24264068711929,0.,2.75735931288071));
#8478=CARTESIAN_POINT('',(3.93914086658804,8.38883057415937E-17,3.02959542363754));
#8479=CARTESIAN_POINT('',(3.71993776442021,-8.38883057415937E-17,3.24879852580537));
#8480=CARTESIAN_POINT('Origin',(3.45477272147525,0.,2.54522727852475));
#8481=CARTESIAN_POINT('Origin',(-0.151471862576143,0.,6.15147186257614));
#8482=CARTESIAN_POINT('',(0.555634918610405,-1.22464679914735E-16,6.85857864376269));
#8483=CARTESIAN_POINT('Origin',(-0.151471862576143,0.,6.15147186257614));
#8484=CARTESIAN_POINT('',(0.555634918610405,-1.22464679914735E-16,6.85857864376269));
#8485=CARTESIAN_POINT('',(0.555634918610405,-1.22464679914735E-16,6.85857864376269));
#8486=CARTESIAN_POINT('',(0.555634918610405,-1.22464679914735E-16,6.85857864376269));
#8487=CARTESIAN_POINT('',(0.555634918610405,-1.22464679914735E-16,6.85857864376269));
#8488=CARTESIAN_POINT('',(0.555634918610405,-1.22464679914735E-16,6.85857864376269));
#8489=CARTESIAN_POINT('',(0.555634918610405,-1.22464679914735E-16,6.85857864376269));
#8490=CARTESIAN_POINT('',(3.94974746830583,-1.22464679914735E-16,3.46446609406726));
#8491=CARTESIAN_POINT('',(0.555634918610405,-1.22464679914735E-16,6.85857864376269));
#8492=CARTESIAN_POINT('Origin',(3.24264068711929,0.,2.75735931288071));
#8493=CARTESIAN_POINT('Origin',(3.24264068711929,0.,2.75735931288071));
#8494=CARTESIAN_POINT('Origin',(-0.151471862576143,0.,6.15147186257614));
#8495=CARTESIAN_POINT('',(0.414213562373095,-9.79717439317883E-17,6.71715728752538));
#8496=CARTESIAN_POINT('Origin',(-0.151471862576143,0.,6.15147186257614));
#8497=CARTESIAN_POINT('Origin',(-0.950502525316942,0.,6.95050252531694));
#8498=CARTESIAN_POINT('',(-0.377746032555838,-9.79717439317883E-17,7.50911688245431));
#8499=CARTESIAN_POINT('Origin',(-0.943431457505076,0.,6.94343145750508));
#8500=CARTESIAN_POINT('',(-0.384817100367704,-9.79717439317883E-17,7.51618795026618));
#8501=CARTESIAN_POINT('Origin',(-0.307035354437183,0.,6.30703535443718));
#8502=CARTESIAN_POINT('',(4.23259018078045,-1.34711147906209E-16,3.32304473782995));
#8503=CARTESIAN_POINT('Origin',(3.45477272147525,0.,2.54522727852475));
#8504=CARTESIAN_POINT('',(0.470782104868019,-1.34711147906209E-16,7.08485281374239));
#8505=CARTESIAN_POINT('',(0.470782104868019,-1.34711147906209E-16,7.08485281374239));
#8506=CARTESIAN_POINT('',(0.470782104868019,-1.34711147906209E-16,7.08485281374239));
#8507=CARTESIAN_POINT('',(0.470782104868019,-1.34711147906209E-16,7.08485281374239));
#8508=CARTESIAN_POINT('',(0.470782104868019,-1.34711147906209E-16,7.08485281374239));
#8509=CARTESIAN_POINT('',(0.470782104868019,-1.34711147906209E-16,7.08485281374239));
#8510=CARTESIAN_POINT('',(0.470782104868019,-1.34711147906209E-16,7.08485281374239));
#8511=CARTESIAN_POINT('',(0.470782104868019,-1.34711147906209E-16,7.08485281374239));
#8512=CARTESIAN_POINT('Origin',(-0.307035354437183,0.,6.30703535443718));
#8513=CARTESIAN_POINT('Origin',(3.45477272147525,0.,2.54522727852475));
#8514=CARTESIAN_POINT('Origin',(-0.519167388793148,0.,6.51916738879315));
#8515=CARTESIAN_POINT('',(0.470782104868019,-1.71450551880629E-16,7.50911688245431));
#8516=CARTESIAN_POINT('Origin',(-0.519167388793148,0.,6.51916738879315));
#8517=CARTESIAN_POINT('',(0.1879393923934,1.22464679914735E-16,7.2262741699797));
#8518=CARTESIAN_POINT('Origin',(-0.519167388793147,0.,6.51916738879315));
#8519=CARTESIAN_POINT('Origin',(-0.519167388793148,0.,6.51916738879315));
#8520=CARTESIAN_POINT('',(0.682914139223983,-1.71450551880629E-16,7.29698484809835));
#8521=CARTESIAN_POINT('Origin',(-0.307035354437183,0.,6.30703535443718));
#8522=CARTESIAN_POINT('',(0.470782104868019,-1.71450551880629E-16,7.50911688245431));
#8523=CARTESIAN_POINT('Origin',(-0.943431457505076,0.,6.94343145750508));
#8524=CARTESIAN_POINT('',(-0.236324676318529,-1.22464679914735E-16,7.65053823869162));
#8525=CARTESIAN_POINT('',(-0.236324676318529,-1.22464679914735E-16,7.65053823869162));
#8526=CARTESIAN_POINT('Origin',(-0.943431457505076,0.,6.94343145750508));
#8527=CARTESIAN_POINT('Origin',(-0.307035354437183,0.,6.30703535443718));
#8528=CARTESIAN_POINT('Origin',(-0.943431457505076,0.,6.94343145750508));
#8529=CARTESIAN_POINT('',(0.,0.,0.));
#8530=CARTESIAN_POINT('Origin',(-0.575735931288071,0.,6.57573593128807));
#8531=CARTESIAN_POINT('',(0.195010460205266,-1.23689326713883E-16,7.23334523779156));
#8532=CARTESIAN_POINT('Origin',(-0.519167388793147,0.,6.51916738879315));
#8533=CARTESIAN_POINT('',(0.138441917710342,-1.23689326713883E-16,7.28991378028648));
#8534=CARTESIAN_POINT('',(0.138441917710342,-1.23689326713883E-16,7.28991378028648));
#8535=CARTESIAN_POINT('Origin',(-0.575735931288071,0.,6.57573593128807));
#8536=CARTESIAN_POINT('Origin',(-0.575735931288071,0.,6.57573593128807));
#8537=CARTESIAN_POINT('',(0.470782104868019,-1.71450551880629E-16,7.50911688245431));
#8538=CARTESIAN_POINT('Origin',(-0.519167388793147,0.,6.51916738879315));
#8539=CARTESIAN_POINT('',(0.414213562373095,-1.71450551880629E-16,7.56568542494924));
#8540=CARTESIAN_POINT('',(0.414213562373095,-1.71450551880629E-16,7.56568542494924));
#8541=CARTESIAN_POINT('Origin',(-0.575735931288071,0.,6.57573593128807));
#8542=CARTESIAN_POINT('Origin',(-0.519167388793147,0.,6.51916738879315));
#8543=CARTESIAN_POINT('Origin',(-0.575735931288071,0.,6.57573593128807));
#8544=CARTESIAN_POINT('',(0.,0.,0.));
#8545=CARTESIAN_POINT('Origin',(3.45477272147525,0.,2.54522727852475));
#8546=CARTESIAN_POINT('',(4.00985154470669,-8.38883057415937E-17,2.95888474551888));
#8547=CARTESIAN_POINT('Origin',(3.5254833995939,0.,2.4745166004061));
#8548=CARTESIAN_POINT('',(3.93914086658804,-8.38883057415937E-17,3.02959542363754));
#8549=CARTESIAN_POINT('',(3.93914086658804,-8.38883057415937E-17,3.02959542363754));
#8550=CARTESIAN_POINT('Origin',(3.45477272147525,0.,2.54522727852475));
#8551=CARTESIAN_POINT('Origin',(3.45477272147525,0.,2.54522727852475));
#8552=CARTESIAN_POINT('',(4.30330085889911,-1.34711147906209E-16,3.2523340597113));
#8553=CARTESIAN_POINT('Origin',(3.5254833995939,0.,2.4745166004061));
#8554=CARTESIAN_POINT('',(4.23259018078045,-1.34711147906209E-16,3.32304473782995));
#8555=CARTESIAN_POINT('',(4.23259018078045,-1.34711147906209E-16,3.32304473782995));
#8556=CARTESIAN_POINT('Origin',(3.45477272147525,0.,2.54522727852475));
#8557=CARTESIAN_POINT('Origin',(3.5254833995939,0.,2.4745166004061));
#8558=CARTESIAN_POINT('Origin',(3.45477272147525,0.,2.54522727852475));
#8559=CARTESIAN_POINT('',(0.,0.,0.));
#8560=CARTESIAN_POINT('Origin',(5.07903679018718,-1.69705627484771,3.32096320981282));
#8561=CARTESIAN_POINT('',(5.38309270609739,-1.69705627484771,3.48359776948573));
#8562=CARTESIAN_POINT('Origin',(5.14974746830583,-1.69705627484771,3.25025253169417));
#8563=CARTESIAN_POINT('',(5.45380338421605,-1.69705627484771,3.41288709136707));
#8564=CARTESIAN_POINT('',(5.31238202797874,-1.69705627484771,3.55430844760438));
#8565=CARTESIAN_POINT('Origin',(5.22045814642449,-1.69705627484771,3.17954185357551));
#8566=CARTESIAN_POINT('Origin',(5.07903679018718,1.69705627484771,3.32096320981282));
#8567=CARTESIAN_POINT('',(5.38309270609739,1.69705627484771,3.48359776948573));
#8568=CARTESIAN_POINT('Origin',(5.14974746830583,1.69705627484771,3.25025253169417));
#8569=CARTESIAN_POINT('',(5.45380338421605,1.69705627484771,3.41288709136707));
#8570=CARTESIAN_POINT('',(5.31238202797874,1.69705627484771,3.55430844760438));
#8571=CARTESIAN_POINT('Origin',(5.22045814642449,1.69705627484771,3.17954185357551));
#8572=CARTESIAN_POINT('Origin',(2.67903679018718,1.69705627484771,0.920963209812822));
#8573=CARTESIAN_POINT('',(2.98309270609739,1.69705627484771,1.08359776948573));
#8574=CARTESIAN_POINT('Origin',(2.74974746830583,1.69705627484771,0.850252531694168));
#8575=CARTESIAN_POINT('',(3.05380338421605,1.69705627484771,1.01288709136707));
#8576=CARTESIAN_POINT('',(2.91238202797874,1.69705627484771,1.15430844760438));
#8577=CARTESIAN_POINT('Origin',(2.82045814642449,1.69705627484771,0.779541853575513));
#8578=CARTESIAN_POINT('Origin',(2.67903679018718,-1.69705627484771,0.920963209812822));
#8579=CARTESIAN_POINT('',(2.98309270609739,-1.69705627484771,1.08359776948573));
#8580=CARTESIAN_POINT('Origin',(2.74974746830583,-1.69705627484771,0.850252531694168));
#8581=CARTESIAN_POINT('',(3.05380338421605,-1.69705627484771,1.01288709136707));
#8582=CARTESIAN_POINT('',(2.91238202797874,-1.69705627484771,1.15430844760438));
#8583=CARTESIAN_POINT('Origin',(2.82045814642449,-1.69705627484771,0.779541853575513));
#8584=CARTESIAN_POINT('Origin',(3.94974746830583,0.,2.05025253169417));
#8585=CARTESIAN_POINT('',(5.15182899632296,-1.95943487863577E-16,3.11091270347399));
#8586=CARTESIAN_POINT('Origin',(4.02045814642449,0.,1.97954185357551));
#8587=CARTESIAN_POINT('',(5.08111831820431,-1.95943487863577E-16,3.18162338159264));
#8588=CARTESIAN_POINT('',(5.08111831820431,-1.95943487863577E-16,3.18162338159264));
#8589=CARTESIAN_POINT('Origin',(3.94974746830583,0.,2.05025253169417));
#8590=CARTESIAN_POINT('Origin',(3.94974746830583,0.,2.05025253169417));
#8591=CARTESIAN_POINT('',(6.14177848998413,-3.67394039744206E-16,4.10086219713516));
#8592=CARTESIAN_POINT('Origin',(4.02045814642449,0.,1.97954185357551));
#8593=CARTESIAN_POINT('',(6.07106781186548,-3.67394039744206E-16,4.17157287525381));
#8594=CARTESIAN_POINT('',(6.07106781186548,-3.67394039744206E-16,4.17157287525381));
#8595=CARTESIAN_POINT('Origin',(3.94974746830583,0.,2.05025253169417));
#8596=CARTESIAN_POINT('Origin',(4.02045814642449,0.,1.97954185357551));
#8597=CARTESIAN_POINT('Origin',(3.94974746830583,0.,2.05025253169417));
#8598=CARTESIAN_POINT('',(0.,0.,0.));
#8599=CARTESIAN_POINT('Origin',(5.14974746830583,-1.69705627484771,3.25025253169417));
#8600=CARTESIAN_POINT('',(5.45380338421605,-1.69705627484771,3.41288709136707));
#8601=CARTESIAN_POINT('Origin',(5.22045814642449,-1.69705627484771,3.17954185357551));
#8602=CARTESIAN_POINT('',(6.1609101654026,-1.69705627484771,2.70578031018053));
#8603=CARTESIAN_POINT('',(5.38309270609739,-1.69705627484771,3.48359776948573));
#8604=CARTESIAN_POINT('Origin',(5.92756492761104,-1.69705627484771,2.47243507238896));
#8605=CARTESIAN_POINT('Origin',(5.14974746830583,1.69705627484771,3.25025253169417));
#8606=CARTESIAN_POINT('',(5.45380338421605,1.69705627484771,3.41288709136707));
#8607=CARTESIAN_POINT('Origin',(5.22045814642449,1.69705627484771,3.17954185357551));
#8608=CARTESIAN_POINT('',(6.1609101654026,1.69705627484771,2.70578031018053));
#8609=CARTESIAN_POINT('',(5.38309270609739,1.69705627484771,3.48359776948573));
#8610=CARTESIAN_POINT('Origin',(5.92756492761104,1.69705627484771,2.47243507238896));
#8611=CARTESIAN_POINT('Origin',(2.74974746830583,1.69705627484771,0.850252531694168));
#8612=CARTESIAN_POINT('',(3.05380338421605,1.69705627484771,1.01288709136707));
#8613=CARTESIAN_POINT('Origin',(2.82045814642449,1.69705627484771,0.779541853575513));
#8614=CARTESIAN_POINT('',(3.7609101654026,1.69705627484771,0.305780310180525));
#8615=CARTESIAN_POINT('',(2.98309270609739,1.69705627484771,1.08359776948573));
#8616=CARTESIAN_POINT('Origin',(3.52756492761104,1.69705627484771,0.0724350723889646));
#8617=CARTESIAN_POINT('Origin',(2.74974746830583,-1.69705627484771,0.850252531694168));
#8618=CARTESIAN_POINT('',(3.05380338421605,-1.69705627484771,1.01288709136707));
#8619=CARTESIAN_POINT('Origin',(2.82045814642449,-1.69705627484771,0.779541853575513));
#8620=CARTESIAN_POINT('',(3.7609101654026,-1.69705627484771,0.305780310180525));
#8621=CARTESIAN_POINT('',(2.98309270609739,-1.69705627484771,1.08359776948573));
#8622=CARTESIAN_POINT('Origin',(3.52756492761104,-1.69705627484771,0.0724350723889646));
#8623=CARTESIAN_POINT('Origin',(3.45477272147525,0.,2.54522727852475));
#8624=CARTESIAN_POINT('',(4.00985154470669,-8.38883057415937E-17,2.95888474551888));
#8625=CARTESIAN_POINT('Origin',(3.5254833995939,0.,2.4745166004061));
#8626=CARTESIAN_POINT('',(5.21193307272382,8.38883057415937E-17,1.75680321750175));
#8627=CARTESIAN_POINT('',(3.93914086658804,-8.38883057415937E-17,3.02959542363754));
#8628=CARTESIAN_POINT('Origin',(4.72756492761104,0.,1.27243507238896));
#8629=CARTESIAN_POINT('Origin',(3.5254833995939,0.,2.4745166004061));
#8630=CARTESIAN_POINT('',(4.939696961967,-1.59204083889156E-16,2.89878066911802));
#8631=CARTESIAN_POINT('Origin',(4.02045814642449,0.,1.97954185357551));
#8632=CARTESIAN_POINT('',(4.44472221513642,-1.59204083889156E-16,3.39375541594861));
#8633=CARTESIAN_POINT('',(4.44472221513642,-1.59204083889156E-16,3.39375541594861));
#8634=CARTESIAN_POINT('Origin',(3.5254833995939,0.,2.4745166004061));
#8635=CARTESIAN_POINT('Origin',(3.5254833995939,0.,2.4745166004061));
#8636=CARTESIAN_POINT('Origin',(4.02045814642449,0.,1.97954185357551));
#8637=CARTESIAN_POINT('',(6.84888527117068,-3.67394039744206E-16,3.39375541594861));
#8638=CARTESIAN_POINT('Origin',(4.72756492761104,0.,1.27243507238896));
#8639=CARTESIAN_POINT('',(6.14177848998413,-3.67394039744206E-16,4.10086219713516));
#8640=CARTESIAN_POINT('',(6.14177848998413,-3.67394039744206E-16,4.10086219713516));
#8641=CARTESIAN_POINT('Origin',(4.02045814642449,0.,1.97954185357551));
#8642=CARTESIAN_POINT('Origin',(4.72756492761104,0.,1.27243507238896));
#8643=CARTESIAN_POINT('Origin',(4.02045814642449,0.,1.97954185357551));
#8644=CARTESIAN_POINT('',(0.,0.,0.));
#8645=CARTESIAN_POINT('Origin',(0.45,0.6,0.));
#8646=CARTESIAN_POINT('',(-0.45,0.6,-5.51091059616309E-17));
#8647=CARTESIAN_POINT('Origin',(0.,0.6,0.));
#8648=CARTESIAN_POINT('Origin',(0.,0.575,0.));
#8649=CARTESIAN_POINT('',(-0.5,0.55,-6.12323399573677E-17));
#8650=CARTESIAN_POINT('Origin',(0.,0.55,0.));
#8651=CARTESIAN_POINT('',(-0.475,0.575,-5.81707229594993E-17));
#8652=CARTESIAN_POINT('Origin',(0.,0.29,0.));
#8653=CARTESIAN_POINT('',(-0.5,0.0299999999999998,-6.12323399573677E-17));
#8654=CARTESIAN_POINT('Origin',(0.,0.0299999999999998,0.));
#8655=CARTESIAN_POINT('',(-0.5,0.29,-6.12323399573677E-17));
#8656=CARTESIAN_POINT('Origin',(0.,0.0150000000000001,0.));
#8657=CARTESIAN_POINT('',(-0.47,7.11236625150491E-17,-5.75583995599256E-17));
#8658=CARTESIAN_POINT('Origin',(0.,0.,0.));
#8659=CARTESIAN_POINT('',(-0.485,0.0150000000000001,-5.93953697586466E-17));
#8660=CARTESIAN_POINT('Origin',(0.32,0.,0.));
#8661=CARTESIAN_POINT('',(-0.32,-6.93889390390723E-18,-3.91886975727153E-17));
#8662=CARTESIAN_POINT('Origin',(0.,0.,0.));
#8663=CARTESIAN_POINT('Origin',(0.,-0.02,0.));
#8664=CARTESIAN_POINT('',(-0.2942,-0.0515999999999999,3.60291088309151E-17));
#8665=CARTESIAN_POINT('Origin',(0.,-0.0515999999999999,0.));
#8666=CARTESIAN_POINT('',(-0.31,-0.02,-3.7964050773568E-17));
#8667=CARTESIAN_POINT('Origin',(0.,-1.24,0.));
#8668=CARTESIAN_POINT('',(-0.2942,-2.4458,3.60291088309151E-17));
#8669=CARTESIAN_POINT('Origin',(0.,-2.4458,0.));
#8670=CARTESIAN_POINT('',(-0.2942,-1.24,-3.60291088309151E-17));
#8671=CARTESIAN_POINT('Origin',(0.,-2.47,0.));
#8672=CARTESIAN_POINT('',(-0.24,-2.5,-2.93915231795365E-17));
#8673=CARTESIAN_POINT('Origin',(0.,-2.5,0.));
#8674=CARTESIAN_POINT('',(-0.27,-2.47,-3.30654635769785E-17));
#8675=CARTESIAN_POINT('Origin',(0.,-2.5,0.));
#8676=CARTESIAN_POINT('Origin',(0.144337567297406,-0.6,-0.25));
#8677=CARTESIAN_POINT('',(0.288675134594813,-0.6,0.));
#8678=CARTESIAN_POINT('',(0.144337567297406,-0.6,-0.25));
#8679=CARTESIAN_POINT('',(0.288675134594813,-0.6,0.));
#8680=CARTESIAN_POINT('',(0.144337567297406,-0.96,-0.25));
#8681=CARTESIAN_POINT('',(0.144337567297406,-0.6,-0.25));
#8682=CARTESIAN_POINT('',(0.288675134594813,-0.96,0.));
#8683=CARTESIAN_POINT('',(0.288675134594813,-0.96,0.));
#8684=CARTESIAN_POINT('',(0.288675134594813,-0.6,0.));
#8685=CARTESIAN_POINT('Origin',(-0.144337567297406,-0.6,-0.25));
#8686=CARTESIAN_POINT('',(-0.144337567297406,-0.6,-0.25));
#8687=CARTESIAN_POINT('',(0.144337567297406,-0.6,-0.25));
#8688=CARTESIAN_POINT('',(-0.144337567297406,-0.96,-0.25));
#8689=CARTESIAN_POINT('',(-0.144337567297406,-0.6,-0.25));
#8690=CARTESIAN_POINT('',(0.144337567297406,-0.96,-0.25));
#8691=CARTESIAN_POINT('Origin',(-0.288675134594813,-0.6,-8.32667268468867E-17));
#8692=CARTESIAN_POINT('',(-0.288675134594813,-0.6,-3.53525079574969E-17));
#8693=CARTESIAN_POINT('',(-0.144337567297406,-0.6,-0.25));
#8694=CARTESIAN_POINT('',(-0.288675134594813,-0.96,-5.55111512312578E-17));
#8695=CARTESIAN_POINT('',(-0.288675134594813,-0.6,-3.53525079574969E-17));
#8696=CARTESIAN_POINT('',(-0.144337567297406,-0.96,-0.25));
#8697=CARTESIAN_POINT('Origin',(-0.144337567297407,-0.6,0.25));
#8698=CARTESIAN_POINT('',(-0.144337567297407,-0.6,0.25));
#8699=CARTESIAN_POINT('',(-0.288675134594813,-0.6,-3.53525079574969E-17));
#8700=CARTESIAN_POINT('',(-0.144337567297407,-0.96,0.25));
#8701=CARTESIAN_POINT('',(-0.144337567297407,-0.6,0.25));
#8702=CARTESIAN_POINT('',(-0.288675134594813,-0.96,-3.53525079574969E-17));
#8703=CARTESIAN_POINT('Origin',(0.144337567297406,-0.6,0.25));
#8704=CARTESIAN_POINT('',(0.144337567297406,-0.6,0.25));
#8705=CARTESIAN_POINT('',(-0.144337567297407,-0.6,0.25));
#8706=CARTESIAN_POINT('',(0.144337567297406,-0.96,0.25));
#8707=CARTESIAN_POINT('',(0.144337567297406,-0.6,0.25));
#8708=CARTESIAN_POINT('',(-0.144337567297407,-0.96,0.25));
#8709=CARTESIAN_POINT('Origin',(0.288675134594813,-0.6,0.));
#8710=CARTESIAN_POINT('',(0.144337567297406,-0.6,0.25));
#8711=CARTESIAN_POINT('',(0.144337567297406,-0.96,0.25));
#8712=CARTESIAN_POINT('Origin',(0.,-0.6,0.));
#8713=CARTESIAN_POINT('Origin',(0.,-0.96,0.));
#8714=CARTESIAN_POINT('',(0.,0.,0.));
#8715=CARTESIAN_POINT('Origin',(0.,-0.6,0.));
#8716=CARTESIAN_POINT('',(1.55884572681199,-0.6,0.));
#8717=CARTESIAN_POINT('',(0.779422863405995,-0.6,1.35));
#8718=CARTESIAN_POINT('',(0.779422863405995,-0.6,1.35));
#8719=CARTESIAN_POINT('',(-0.779422863405996,-0.6,1.35));
#8720=CARTESIAN_POINT('',(-0.779422863405996,-0.6,1.35));
#8721=CARTESIAN_POINT('',(-1.55884572681199,-0.6,-1.90903542970483E-16));
#8722=CARTESIAN_POINT('',(-1.55884572681199,-0.6,-1.90903542970483E-16));
#8723=CARTESIAN_POINT('',(-0.779422863405995,-0.6,-1.35));
#8724=CARTESIAN_POINT('',(-0.779422863405995,-0.6,-1.35));
#8725=CARTESIAN_POINT('',(0.779422863405995,-0.6,-1.35));
#8726=CARTESIAN_POINT('',(0.779422863405995,-0.6,-1.35));
#8727=CARTESIAN_POINT('',(1.55884572681199,-0.6,0.));
#8728=CARTESIAN_POINT('',(-1.065,-0.6,-1.30424884109193E-16));
#8729=CARTESIAN_POINT('Origin',(0.,-0.6,0.));
#8730=CARTESIAN_POINT('Origin',(0.,0.6,0.));
#8731=CARTESIAN_POINT('',(0.779422863405995,0.6,1.35));
#8732=CARTESIAN_POINT('',(1.55884572681199,0.6,0.));
#8733=CARTESIAN_POINT('',(0.779422863405995,0.6,1.35));
#8734=CARTESIAN_POINT('',(0.779422863405995,0.6,-1.35));
#8735=CARTESIAN_POINT('',(1.55884572681199,0.6,0.));
#8736=CARTESIAN_POINT('',(-0.779422863405995,0.6,-1.35));
#8737=CARTESIAN_POINT('',(0.779422863405995,0.6,-1.35));
#8738=CARTESIAN_POINT('',(-1.55884572681199,0.6,-1.90903542970483E-16));
#8739=CARTESIAN_POINT('',(-0.779422863405995,0.6,-1.35));
#8740=CARTESIAN_POINT('',(-0.779422863405996,0.6,1.35));
#8741=CARTESIAN_POINT('',(-1.55884572681199,0.6,-1.90903542970483E-16));
#8742=CARTESIAN_POINT('',(-0.779422863405996,0.6,1.35));
#8743=CARTESIAN_POINT('',(-1.065,0.6,1.30424884109193E-16));
#8744=CARTESIAN_POINT('Origin',(0.,0.6,0.));
#8745=CARTESIAN_POINT('Origin',(-0.779422863405996,0.,1.35));
#8746=CARTESIAN_POINT('',(0.779422863405995,0.,1.35));
#8747=CARTESIAN_POINT('',(-0.779422863405996,0.,1.35));
#8748=CARTESIAN_POINT('Origin',(-1.55884572681199,0.,-1.90903542970483E-16));
#8749=CARTESIAN_POINT('',(-1.55884572681199,0.,-1.90903542970483E-16));
#8750=CARTESIAN_POINT('Origin',(-0.779422863405995,0.,-1.35));
#8751=CARTESIAN_POINT('',(-0.779422863405995,0.,-1.35));
#8752=CARTESIAN_POINT('Origin',(0.779422863405995,0.,-1.35));
#8753=CARTESIAN_POINT('',(0.779422863405995,0.,-1.35));
#8754=CARTESIAN_POINT('Origin',(1.55884572681199,0.,0.));
#8755=CARTESIAN_POINT('',(1.55884572681199,0.,0.));
#8756=CARTESIAN_POINT('Origin',(0.779422863405995,0.,1.35));
#8757=CARTESIAN_POINT('Origin',(0.,0.,0.));
#8758=CARTESIAN_POINT('',(-1.065,2.47,-1.30424884109193E-16));
#8759=CARTESIAN_POINT('',(-1.065,0.,-1.30424884109193E-16));
#8760=CARTESIAN_POINT('Origin',(0.,2.47,0.));
#8761=CARTESIAN_POINT('Origin',(0.985,2.55,0.));
#8762=CARTESIAN_POINT('',(-0.985,2.55,-1.20627709716014E-16));
#8763=CARTESIAN_POINT('Origin',(0.,2.55,0.));
#8764=CARTESIAN_POINT('',(-0.79,2.55,-9.67470971326409E-17));
#8765=CARTESIAN_POINT('Origin',(0.,2.55,0.));
#8766=CARTESIAN_POINT('Origin',(0.,2.51,0.));
#8767=CARTESIAN_POINT('',(-1.025,2.51,-1.25526296912604E-16));
#8768=CARTESIAN_POINT('Origin',(0.,0.,0.));
#8769=CARTESIAN_POINT('',(-1.065,-2.47,-1.30424884109193E-16));
#8770=CARTESIAN_POINT('Origin',(0.,-2.47,0.));
#8771=CARTESIAN_POINT('',(-1.065,0.,-1.30424884109193E-16));
#8772=CARTESIAN_POINT('Origin',(0.,-2.51,0.));
#8773=CARTESIAN_POINT('',(-0.985,-2.55,-1.20627709716014E-16));
#8774=CARTESIAN_POINT('Origin',(0.,-2.55,0.));
#8775=CARTESIAN_POINT('',(-1.025,-2.51,-1.25526296912604E-16));
#8776=CARTESIAN_POINT('Origin',(0.79,-2.55,0.));
#8777=CARTESIAN_POINT('',(-0.79,-2.55,-9.67470971326409E-17));
#8778=CARTESIAN_POINT('Origin',(0.,-2.55,0.));
#8779=CARTESIAN_POINT('Origin',(0.,0.,0.));
#8780=CARTESIAN_POINT('',(-0.79,0.,-9.67470971326409E-17));
#8781=CARTESIAN_POINT('',(0.,0.,0.));
#8782=CARTESIAN_POINT('Origin',(5.5,0.,3.5));
#8783=CARTESIAN_POINT('',(5.5,0.505181485540923,2.625));
#8784=CARTESIAN_POINT('',(5.5,1.01036297108185,3.5));
#8785=CARTESIAN_POINT('',(5.5,0.505181485540923,2.625));
#8786=CARTESIAN_POINT('',(5.5,-0.505181485540923,2.625));
#8787=CARTESIAN_POINT('',(5.5,-0.505181485540923,2.625));
#8788=CARTESIAN_POINT('',(5.5,-1.01036297108185,3.5));
#8789=CARTESIAN_POINT('',(5.5,-1.01036297108185,3.5));
#8790=CARTESIAN_POINT('',(5.5,-0.505181485540922,4.375));
#8791=CARTESIAN_POINT('',(5.5,-0.505181485540922,4.375));
#8792=CARTESIAN_POINT('',(5.5,0.505181485540923,4.375));
#8793=CARTESIAN_POINT('',(5.5,0.505181485540923,4.375));
#8794=CARTESIAN_POINT('',(5.5,1.01036297108185,3.5));
#8795=CARTESIAN_POINT('',(5.5,-8.38883057415937E-17,4.185));
#8796=CARTESIAN_POINT('Origin',(5.5,0.,3.5));
#8797=CARTESIAN_POINT('Origin',(5.5,-0.505181485540923,2.625));
#8798=CARTESIAN_POINT('',(6.1,0.505181485540923,2.625));
#8799=CARTESIAN_POINT('',(5.5,0.505181485540923,2.625));
#8800=CARTESIAN_POINT('',(6.1,-0.505181485540923,2.625));
#8801=CARTESIAN_POINT('',(6.1,-0.505181485540923,2.625));
#8802=CARTESIAN_POINT('',(5.5,-0.505181485540923,2.625));
#8803=CARTESIAN_POINT('Origin',(5.5,-1.01036297108185,3.5));
#8804=CARTESIAN_POINT('',(6.1,-1.01036297108185,3.5));
#8805=CARTESIAN_POINT('',(6.1,-1.01036297108185,3.5));
#8806=CARTESIAN_POINT('',(5.5,-1.01036297108185,3.5));
#8807=CARTESIAN_POINT('Origin',(5.5,-0.505181485540922,4.375));
#8808=CARTESIAN_POINT('',(6.1,-0.505181485540922,4.375));
#8809=CARTESIAN_POINT('',(6.1,-0.505181485540922,4.375));
#8810=CARTESIAN_POINT('',(5.5,-0.505181485540922,4.375));
#8811=CARTESIAN_POINT('Origin',(5.5,0.505181485540923,4.375));
#8812=CARTESIAN_POINT('',(6.1,0.505181485540923,4.375));
#8813=CARTESIAN_POINT('',(6.1,0.505181485540923,4.375));
#8814=CARTESIAN_POINT('',(5.5,0.505181485540923,4.375));
#8815=CARTESIAN_POINT('Origin',(5.5,1.01036297108185,3.5));
#8816=CARTESIAN_POINT('',(6.1,1.01036297108185,3.5));
#8817=CARTESIAN_POINT('',(6.1,1.01036297108185,3.5));
#8818=CARTESIAN_POINT('',(5.5,1.01036297108185,3.5));
#8819=CARTESIAN_POINT('Origin',(5.5,0.505181485540923,2.625));
#8820=CARTESIAN_POINT('',(6.1,0.505181485540923,2.625));
#8821=CARTESIAN_POINT('Origin',(6.1,0.,3.5));
#8822=CARTESIAN_POINT('Origin',(4.1,0.,3.5));
#8823=CARTESIAN_POINT('',(4.1,-8.38883057415937E-17,4.185));
#8824=CARTESIAN_POINT('',(4.1,-8.38883057415937E-17,4.185));
#8825=CARTESIAN_POINT('Origin',(4.1,0.,3.5));
#8826=CARTESIAN_POINT('Origin',(4.1,0.,3.5));
#8827=CARTESIAN_POINT('',(0.,0.,0.));
#8828=CARTESIAN_POINT('',(0.,0.,0.));
#8829=CARTESIAN_POINT('',(0.,0.,0.));
#8830=CARTESIAN_POINT('',(0.,0.,0.));
#8831=CARTESIAN_POINT('',(0.,0.,0.));
#8832=CARTESIAN_POINT('',(0.,0.,0.));
#8833=CARTESIAN_POINT('',(3.52756492761104,1.69705627484771,0.0724350723889643));
#8834=CARTESIAN_POINT('',(5.92756492761104,1.69705627484771,2.47243507238896));
#8835=CARTESIAN_POINT('',(5.92756492761104,-1.69705627484771,2.47243507238896));
#8836=CARTESIAN_POINT('',(3.52756492761104,-1.69705627484771,0.0724350723889636));
#8837=CARTESIAN_POINT('',(-5.85,0.,7.));
#8838=CARTESIAN_POINT('',(5.85,0.,7.));
#8839=CARTESIAN_POINT('',(-1.63639610306789,0.,2.68664863476206));
#8840=CARTESIAN_POINT('',(0.,0.,0.));
#8841=UNCERTAINTY_MEASURE_WITH_UNIT(LENGTH_MEASURE(0.001),#8865,
'DISTANCE_ACCURACY_VALUE',
'Maximum model space distance between geometric entities at asserted c
onnectivities');
#8842=UNCERTAINTY_MEASURE_WITH_UNIT(LENGTH_MEASURE(0.001),#8865,
'DISTANCE_ACCURACY_VALUE',
'Maximum model space distance between geometric entities at asserted c
onnectivities');
#8843=UNCERTAINTY_MEASURE_WITH_UNIT(LENGTH_MEASURE(0.001),#8865,
'DISTANCE_ACCURACY_VALUE',
'Maximum model space distance between geometric entities at asserted c
onnectivities');
#8844=UNCERTAINTY_MEASURE_WITH_UNIT(LENGTH_MEASURE(0.001),#8865,
'DISTANCE_ACCURACY_VALUE',
'Maximum model space distance between geometric entities at asserted c
onnectivities');
#8845=UNCERTAINTY_MEASURE_WITH_UNIT(LENGTH_MEASURE(0.001),#8865,
'DISTANCE_ACCURACY_VALUE',
'Maximum model space distance between geometric entities at asserted c
onnectivities');
#8846=UNCERTAINTY_MEASURE_WITH_UNIT(LENGTH_MEASURE(0.001),#8865,
'DISTANCE_ACCURACY_VALUE',
'Maximum model space distance between geometric entities at asserted c
onnectivities');
#8847=UNCERTAINTY_MEASURE_WITH_UNIT(LENGTH_MEASURE(0.001),#8865,
'DISTANCE_ACCURACY_VALUE',
'Maximum model space distance between geometric entities at asserted c
onnectivities');
#8848=UNCERTAINTY_MEASURE_WITH_UNIT(LENGTH_MEASURE(0.001),#8865,
'DISTANCE_ACCURACY_VALUE',
'Maximum model space distance between geometric entities at asserted c
onnectivities');
#8849=UNCERTAINTY_MEASURE_WITH_UNIT(LENGTH_MEASURE(0.001),#8865,
'DISTANCE_ACCURACY_VALUE',
'Maximum model space distance between geometric entities at asserted c
onnectivities');
#8850=UNCERTAINTY_MEASURE_WITH_UNIT(LENGTH_MEASURE(0.001),#8865,
'DISTANCE_ACCURACY_VALUE',
'Maximum model space distance between geometric entities at asserted c
onnectivities');
#8851=UNCERTAINTY_MEASURE_WITH_UNIT(LENGTH_MEASURE(0.001),#8865,
'DISTANCE_ACCURACY_VALUE',
'Maximum model space distance between geometric entities at asserted c
onnectivities');
#8852=UNCERTAINTY_MEASURE_WITH_UNIT(LENGTH_MEASURE(0.001),#8865,
'DISTANCE_ACCURACY_VALUE',
'Maximum model space distance between geometric entities at asserted c
onnectivities');
#8853=(
GEOMETRIC_REPRESENTATION_CONTEXT(3)
GLOBAL_UNCERTAINTY_ASSIGNED_CONTEXT((#8841))
GLOBAL_UNIT_ASSIGNED_CONTEXT((#8865,#8867,#8868))
REPRESENTATION_CONTEXT('','3D')
);
#8854=(
GEOMETRIC_REPRESENTATION_CONTEXT(3)
GLOBAL_UNCERTAINTY_ASSIGNED_CONTEXT((#8842))
GLOBAL_UNIT_ASSIGNED_CONTEXT((#8865,#8867,#8868))
REPRESENTATION_CONTEXT('','3D')
);
#8855=(
GEOMETRIC_REPRESENTATION_CONTEXT(3)
GLOBAL_UNCERTAINTY_ASSIGNED_CONTEXT((#8843))
GLOBAL_UNIT_ASSIGNED_CONTEXT((#8865,#8867,#8868))
REPRESENTATION_CONTEXT('','3D')
);
#8856=(
GEOMETRIC_REPRESENTATION_CONTEXT(3)
GLOBAL_UNCERTAINTY_ASSIGNED_CONTEXT((#8844))
GLOBAL_UNIT_ASSIGNED_CONTEXT((#8865,#8867,#8868))
REPRESENTATION_CONTEXT('','3D')
);
#8857=(
GEOMETRIC_REPRESENTATION_CONTEXT(3)
GLOBAL_UNCERTAINTY_ASSIGNED_CONTEXT((#8845))
GLOBAL_UNIT_ASSIGNED_CONTEXT((#8865,#8867,#8868))
REPRESENTATION_CONTEXT('','3D')
);
#8858=(
GEOMETRIC_REPRESENTATION_CONTEXT(3)
GLOBAL_UNCERTAINTY_ASSIGNED_CONTEXT((#8846))
GLOBAL_UNIT_ASSIGNED_CONTEXT((#8865,#8867,#8868))
REPRESENTATION_CONTEXT('','3D')
);
#8859=(
GEOMETRIC_REPRESENTATION_CONTEXT(3)
GLOBAL_UNCERTAINTY_ASSIGNED_CONTEXT((#8847))
GLOBAL_UNIT_ASSIGNED_CONTEXT((#8865,#8867,#8868))
REPRESENTATION_CONTEXT('','3D')
);
#8860=(
GEOMETRIC_REPRESENTATION_CONTEXT(3)
GLOBAL_UNCERTAINTY_ASSIGNED_CONTEXT((#8848))
GLOBAL_UNIT_ASSIGNED_CONTEXT((#8865,#8867,#8868))
REPRESENTATION_CONTEXT('','3D')
);
#8861=(
GEOMETRIC_REPRESENTATION_CONTEXT(3)
GLOBAL_UNCERTAINTY_ASSIGNED_CONTEXT((#8849))
GLOBAL_UNIT_ASSIGNED_CONTEXT((#8865,#8867,#8868))
REPRESENTATION_CONTEXT('','3D')
);
#8862=(
GEOMETRIC_REPRESENTATION_CONTEXT(3)
GLOBAL_UNCERTAINTY_ASSIGNED_CONTEXT((#8850))
GLOBAL_UNIT_ASSIGNED_CONTEXT((#8865,#8867,#8868))
REPRESENTATION_CONTEXT('','3D')
);
#8863=(
GEOMETRIC_REPRESENTATION_CONTEXT(3)
GLOBAL_UNCERTAINTY_ASSIGNED_CONTEXT((#8851))
GLOBAL_UNIT_ASSIGNED_CONTEXT((#8865,#8867,#8868))
REPRESENTATION_CONTEXT('','3D')
);
#8864=(
GEOMETRIC_REPRESENTATION_CONTEXT(3)
GLOBAL_UNCERTAINTY_ASSIGNED_CONTEXT((#8852))
GLOBAL_UNIT_ASSIGNED_CONTEXT((#8865,#8867,#8868))
REPRESENTATION_CONTEXT('','3D')
);
#8865=(
LENGTH_UNIT()
NAMED_UNIT(*)
SI_UNIT(.CENTI.,.METRE.)
);
#8866=(
LENGTH_UNIT()
NAMED_UNIT(*)
SI_UNIT($,.METRE.)
);
#8867=(
NAMED_UNIT(*)
PLANE_ANGLE_UNIT()
SI_UNIT($,.RADIAN.)
);
#8868=(
NAMED_UNIT(*)
SI_UNIT($,.STERADIAN.)
SOLID_ANGLE_UNIT()
);
#8869=SHAPE_DEFINITION_REPRESENTATION(#8880,#8905);
#8870=SHAPE_DEFINITION_REPRESENTATION(#8881,#8906);
#8871=SHAPE_DEFINITION_REPRESENTATION(#8882,#8907);
#8872=SHAPE_DEFINITION_REPRESENTATION(#8883,#8908);
#8873=SHAPE_DEFINITION_REPRESENTATION(#8884,#8909);
#8874=SHAPE_DEFINITION_REPRESENTATION(#8885,#8910);
#8875=SHAPE_DEFINITION_REPRESENTATION(#8886,#8911);
#8876=SHAPE_DEFINITION_REPRESENTATION(#8887,#8912);
#8877=SHAPE_DEFINITION_REPRESENTATION(#8888,#8913);
#8878=SHAPE_DEFINITION_REPRESENTATION(#8889,#8914);
#8879=SHAPE_DEFINITION_REPRESENTATION(#8890,#8915);
#8880=PRODUCT_DEFINITION_SHAPE('',$,#8917);
#8881=PRODUCT_DEFINITION_SHAPE('',$,#8918);
#8882=PRODUCT_DEFINITION_SHAPE('',$,#8919);
#8883=PRODUCT_DEFINITION_SHAPE('',$,#8920);
#8884=PRODUCT_DEFINITION_SHAPE('',$,#8921);
#8885=PRODUCT_DEFINITION_SHAPE('',$,#8922);
#8886=PRODUCT_DEFINITION_SHAPE('',$,#8923);
#8887=PRODUCT_DEFINITION_SHAPE('',$,#8924);
#8888=PRODUCT_DEFINITION_SHAPE('',$,#8925);
#8889=PRODUCT_DEFINITION_SHAPE('',$,#8926);
#8890=PRODUCT_DEFINITION_SHAPE('',$,#8927);
#8891=PRODUCT_DEFINITION_SHAPE($,$,#53);
#8892=PRODUCT_DEFINITION_SHAPE($,$,#54);
#8893=PRODUCT_DEFINITION_SHAPE($,$,#55);
#8894=PRODUCT_DEFINITION_SHAPE($,$,#56);
#8895=PRODUCT_DEFINITION_SHAPE($,$,#57);
#8896=PRODUCT_DEFINITION_SHAPE($,$,#58);
#8897=PRODUCT_DEFINITION_SHAPE($,$,#59);
#8898=PRODUCT_DEFINITION_SHAPE($,$,#60);
#8899=PRODUCT_DEFINITION_SHAPE($,$,#61);
#8900=PRODUCT_DEFINITION_SHAPE($,$,#62);
#8901=PRODUCT_DEFINITION_SHAPE($,$,#63);
#8902=PRODUCT_DEFINITION_SHAPE($,$,#64);
#8903=PRODUCT_DEFINITION_SHAPE($,$,#65);
#8904=PRODUCT_DEFINITION_SHAPE($,$,#66);
#8905=SHAPE_REPRESENTATION('',(#3493,#3770),#8853);
#8906=SHAPE_REPRESENTATION('',(#3494,#3757,#3758,#3759,#3760,#3761,#3762,
#3763,#3764,#3765,#3766,#3767,#3768,#3769),#8854);
#8907=SHAPE_REPRESENTATION('',(#3495),#8855);
#8908=SHAPE_REPRESENTATION('',(#3557),#8856);
#8909=SHAPE_REPRESENTATION('',(#3630),#8857);
#8910=SHAPE_REPRESENTATION('',(#3639),#8858);
#8911=SHAPE_REPRESENTATION('',(#3648),#8859);
#8912=SHAPE_REPRESENTATION('',(#3669),#8860);
#8913=SHAPE_REPRESENTATION('',(#3694),#8861);
#8914=SHAPE_REPRESENTATION('',(#3720),#8862);
#8915=SHAPE_REPRESENTATION('',(#3744),#8863);
#8916=PRODUCT_DEFINITION_CONTEXT('part definition',#8951,'design');
#8917=PRODUCT_DEFINITION('PAT-125','PAT-125',#8928,#8916);
#8918=PRODUCT_DEFINITION(
'Strainer housing basket seals cap and fittings',
'Strainer housing basket seals cap and fittings',#8929,#8916);
#8919=PRODUCT_DEFINITION('Round-chamber strainer housing',
'Round-chamber strainer housing',#8930,#8916);
#8920=PRODUCT_DEFINITION('Removable cylindrical screen basket',
'Removable cylindrical screen basket',#8931,#8916);
#8921=PRODUCT_DEFINITION('Basket inlet face seal',
'Basket inlet face seal',#8932,#8916);
#8922=PRODUCT_DEFINITION('Basket drain face seal',
'Basket drain face seal',#8933,#8916);
#8923=PRODUCT_DEFINITION('Service cap gasket','Service cap gasket',#8934,
#8916);
#8924=PRODUCT_DEFINITION('Basket-retaining drain cap',
'Basket-retaining drain cap',#8935,#8916);
#8925=PRODUCT_DEFINITION('Cap Screw - M6x25','Cap Screw - M6x25',#8936,
#8916);
#8926=PRODUCT_DEFINITION(
'Hex Pipe Nipple - 1-2 Inch Tapered Pipe Thread',
'Hex Pipe Nipple - 1-2 Inch Tapered Pipe Thread',#8937,#8916);
#8927=PRODUCT_DEFINITION('Blanking plug','Blanking plug',#8938,#8916);
#8928=PRODUCT_DEFINITION_FORMATION('',$,#8953);
#8929=PRODUCT_DEFINITION_FORMATION('',$,#8954);
#8930=PRODUCT_DEFINITION_FORMATION('',$,#8955);
#8931=PRODUCT_DEFINITION_FORMATION('',$,#8956);
#8932=PRODUCT_DEFINITION_FORMATION('',$,#8957);
#8933=PRODUCT_DEFINITION_FORMATION('',$,#8958);
#8934=PRODUCT_DEFINITION_FORMATION('',$,#8959);
#8935=PRODUCT_DEFINITION_FORMATION('',$,#8960);
#8936=PRODUCT_DEFINITION_FORMATION('',$,#8961);
#8937=PRODUCT_DEFINITION_FORMATION('',$,#8962);
#8938=PRODUCT_DEFINITION_FORMATION('',$,#8963);
#8939=PRODUCT_RELATED_PRODUCT_CATEGORY('PAT-125','PAT-125',(#8953));
#8940=PRODUCT_RELATED_PRODUCT_CATEGORY(
'Strainer housing basket seals cap and fittings',
'Strainer housing basket seals cap and fittings',(#8954));
#8941=PRODUCT_RELATED_PRODUCT_CATEGORY('Round-chamber strainer housing',
'Round-chamber strainer housing',(#8955));
#8942=PRODUCT_RELATED_PRODUCT_CATEGORY(
'Removable cylindrical screen basket',
'Removable cylindrical screen basket',(#8956));
#8943=PRODUCT_RELATED_PRODUCT_CATEGORY('Basket inlet face seal',
'Basket inlet face seal',(#8957));
#8944=PRODUCT_RELATED_PRODUCT_CATEGORY('Basket drain face seal',
'Basket drain face seal',(#8958));
#8945=PRODUCT_RELATED_PRODUCT_CATEGORY('Service cap gasket',
'Service cap gasket',(#8959));
#8946=PRODUCT_RELATED_PRODUCT_CATEGORY('Basket-retaining drain cap',
'Basket-retaining drain cap',(#8960));
#8947=PRODUCT_RELATED_PRODUCT_CATEGORY('Cap Screw - M6x25',
'Cap Screw - M6x25',(#8961));
#8948=PRODUCT_RELATED_PRODUCT_CATEGORY(
'Hex Pipe Nipple - 1-2 Inch Tapered Pipe Thread',
'Hex Pipe Nipple - 1-2 Inch Tapered Pipe Thread',(#8962));
#8949=PRODUCT_RELATED_PRODUCT_CATEGORY('Blanking plug','Blanking plug',
(#8963));
#8950=APPLICATION_PROTOCOL_DEFINITION('international standard',
'automotive_design',2009,#8951);
#8951=APPLICATION_CONTEXT(
'Core Data for Automotive Mechanical Design Process');
#8952=PRODUCT_CONTEXT('part definition',#8951,'mechanical');
#8953=PRODUCT('PAT-125','PAT-125',
'PAT-125',(#8952));
#8954=PRODUCT('Strainer housing basket seals cap and fittings',
'Strainer housing basket seals cap and fittings',
'Strainer housing basket seals cap and fittings',(#8952));
#8955=PRODUCT('Round-chamber strainer housing',
'Round-chamber strainer housing','Round-chamber strainer housing',(#8952));
#8956=PRODUCT('Removable cylindrical screen basket',
'Removable cylindrical screen basket',
'Removable cylindrical screen basket',(#8952));
#8957=PRODUCT('Basket inlet face seal','Basket inlet face seal',
'Basket inlet face seal',(#8952));
#8958=PRODUCT('Basket drain face seal','Basket drain face seal',
'Basket drain face seal',(#8952));
#8959=PRODUCT('Service cap gasket','Service cap gasket',
'Service cap gasket',(#8952));
#8960=PRODUCT('Basket-retaining drain cap','Basket-retaining drain cap',
'Basket-retaining drain cap',(#8952));
#8961=PRODUCT('Cap Screw - M6x25','Cap Screw - M6x25',
'Cap Screw - M6x25',(#8952));
#8962=PRODUCT('Hex Pipe Nipple - 1-2 Inch Tapered Pipe Thread',
'Hex Pipe Nipple - 1-2 Inch Tapered Pipe Thread',
'Hex Pipe Nipple - 1-2 Inch Tapered Pipe Thread',(#8952));
#8963=PRODUCT('Blanking plug','Blanking plug','Blanking plug',(#8952));
#8964=PRESENTATION_STYLE_ASSIGNMENT((#8970));
#8965=PRESENTATION_STYLE_ASSIGNMENT((#8971));
#8966=PRESENTATION_STYLE_ASSIGNMENT((#8972));
#8967=PRESENTATION_STYLE_ASSIGNMENT((#8973));
#8968=PRESENTATION_STYLE_ASSIGNMENT((#8974));
#8969=PRESENTATION_STYLE_ASSIGNMENT((#8975));
#8970=SURFACE_STYLE_USAGE(.BOTH.,#8976);
#8971=SURFACE_STYLE_USAGE(.BOTH.,#8977);
#8972=SURFACE_STYLE_USAGE(.BOTH.,#8978);
#8973=SURFACE_STYLE_USAGE(.BOTH.,#8979);
#8974=SURFACE_STYLE_USAGE(.BOTH.,#8980);
#8975=SURFACE_STYLE_USAGE(.BOTH.,#8981);
#8976=SURFACE_SIDE_STYLE('',(#8982));
#8977=SURFACE_SIDE_STYLE('',(#8983));
#8978=SURFACE_SIDE_STYLE('',(#8984));
#8979=SURFACE_SIDE_STYLE('',(#8985));
#8980=SURFACE_SIDE_STYLE('',(#8986));
#8981=SURFACE_SIDE_STYLE('',(#8987));
#8982=SURFACE_STYLE_FILL_AREA(#8988);
#8983=SURFACE_STYLE_FILL_AREA(#8989);
#8984=SURFACE_STYLE_FILL_AREA(#8990);
#8985=SURFACE_STYLE_FILL_AREA(#8991);
#8986=SURFACE_STYLE_FILL_AREA(#8992);
#8987=SURFACE_STYLE_FILL_AREA(#8993);
#8988=FILL_AREA_STYLE('Steel - Satin',(#8994));
#8989=FILL_AREA_STYLE('CAD Library Painted - Light blue',(#8995));
#8990=FILL_AREA_STYLE('CAD Library Painted - Engineering blue',(#8996));
#8991=FILL_AREA_STYLE('CAD Library Painted - Off white',(#8997));
#8992=FILL_AREA_STYLE('CAD Library Painted - Graphite',(#8998));
#8993=FILL_AREA_STYLE('CAD Library Painted - Steel gray',(#8999));
#8994=FILL_AREA_STYLE_COLOUR('Steel - Satin',#9000);
#8995=FILL_AREA_STYLE_COLOUR('CAD Library Painted - Light blue',#9001);
#8996=FILL_AREA_STYLE_COLOUR('CAD Library Painted - Engineering blue',#9002);
#8997=FILL_AREA_STYLE_COLOUR('CAD Library Painted - Off white',#9003);
#8998=FILL_AREA_STYLE_COLOUR('CAD Library Painted - Graphite',#9004);
#8999=FILL_AREA_STYLE_COLOUR('CAD Library Painted - Steel gray',#9005);
#9000=COLOUR_RGB('Steel - Satin',0.627450980392157,0.627450980392157,0.627450980392157);
#9001=COLOUR_RGB('CAD Library Painted - Light blue',0.286274509803922,0.552941176470588,
0.780392156862745);
#9002=COLOUR_RGB('CAD Library Painted - Engineering blue',0.12156862745098,
0.356862745098039,0.6);
#9003=COLOUR_RGB('CAD Library Painted - Off white',0.909803921568627,0.901960784313726,
0.858823529411765);
#9004=COLOUR_RGB('CAD Library Painted - Graphite',0.0980392156862745,0.109803921568627,
0.125490196078431);
#9005=COLOUR_RGB('CAD Library Painted - Steel gray',0.592156862745098,0.631372549019608,
0.67843137254902);
#9006=COLOUR_RGB('Dark Blue',0.08,0.2,0.34);
#9007=FILL_AREA_STYLE_COLOUR('',#9006);
#9008=FILL_AREA_STYLE('',(#9007));
#9009=SURFACE_STYLE_FILL_AREA(#9008);
#9010=SURFACE_SIDE_STYLE('',(#9009));
#9011=SURFACE_STYLE_USAGE(.BOTH.,#9010);
#9012=PRESENTATION_STYLE_ASSIGNMENT((#9011));
#9013=COLOUR_RGB('Light Blue',0.38,0.62,0.78);
#9014=FILL_AREA_STYLE_COLOUR('',#9013);
#9015=FILL_AREA_STYLE('',(#9014));
#9016=SURFACE_STYLE_FILL_AREA(#9015);
#9017=SURFACE_SIDE_STYLE('',(#9016));
#9018=SURFACE_STYLE_USAGE(.BOTH.,#9017);
#9019=PRESENTATION_STYLE_ASSIGNMENT((#9018));
#9020=COLOUR_RGB('Sky Blue',0.24,0.69,0.87);
#9021=FILL_AREA_STYLE_COLOUR('',#9020);
#9022=FILL_AREA_STYLE('',(#9021));
#9023=SURFACE_STYLE_FILL_AREA(#9022);
#9024=SURFACE_SIDE_STYLE('',(#9023));
#9025=SURFACE_STYLE_USAGE(.BOTH.,#9024);
#9026=PRESENTATION_STYLE_ASSIGNMENT((#9025));
#9027=COLOUR_RGB('Grey',0.48,0.52,0.57);
#9028=FILL_AREA_STYLE_COLOUR('',#9027);
#9029=FILL_AREA_STYLE('',(#9028));
#9030=SURFACE_STYLE_FILL_AREA(#9029);
#9031=SURFACE_SIDE_STYLE('',(#9030));
#9032=SURFACE_STYLE_USAGE(.BOTH.,#9031);
#9033=PRESENTATION_STYLE_ASSIGNMENT((#9032));
#9034=COLOUR_RGB('Black',0.12,0.14,0.17);
#9035=FILL_AREA_STYLE_COLOUR('',#9034);
#9036=FILL_AREA_STYLE('',(#9035));
#9037=SURFACE_STYLE_FILL_AREA(#9036);
#9038=SURFACE_SIDE_STYLE('',(#9037));
#9039=SURFACE_STYLE_USAGE(.BOTH.,#9038);
#9040=PRESENTATION_STYLE_ASSIGNMENT((#9039));
#9041=COLOUR_RGB('Off White',0.89,0.88,0.83);
#9042=FILL_AREA_STYLE_COLOUR('',#9041);
#9043=FILL_AREA_STYLE('',(#9042));
#9044=SURFACE_STYLE_FILL_AREA(#9043);
#9045=SURFACE_SIDE_STYLE('',(#9044));
#9046=SURFACE_STYLE_USAGE(.BOTH.,#9045);
#9047=PRESENTATION_STYLE_ASSIGNMENT((#9046));
ENDSEC;
END-ISO-10303-21;
